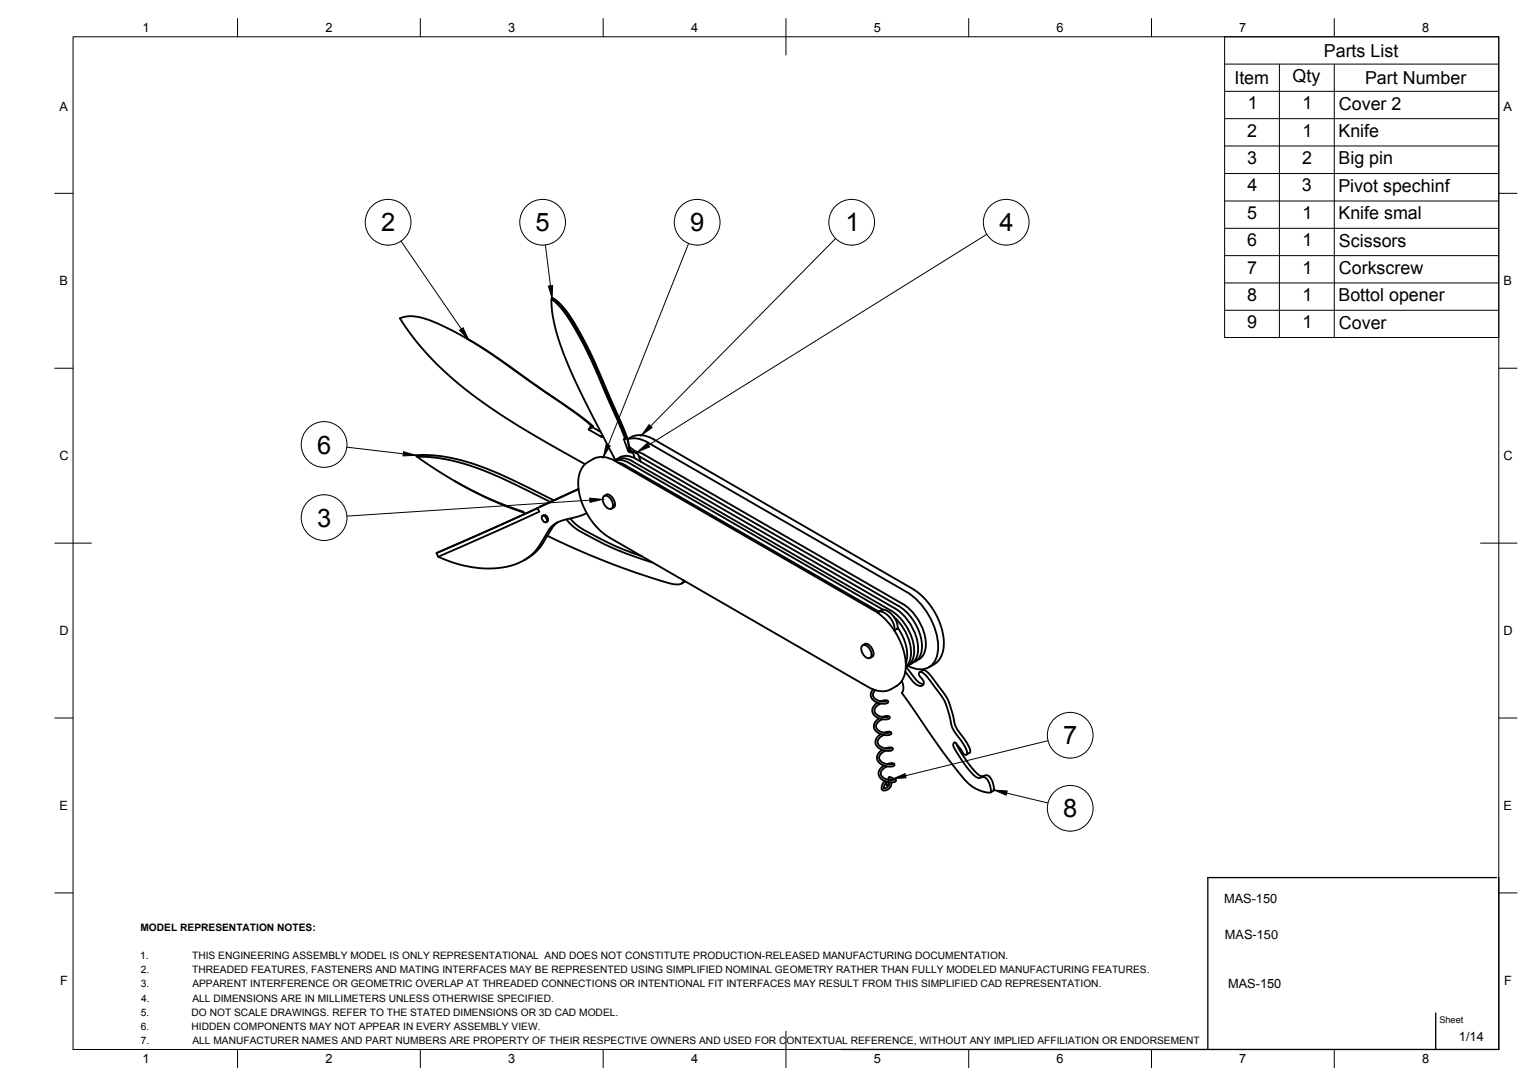
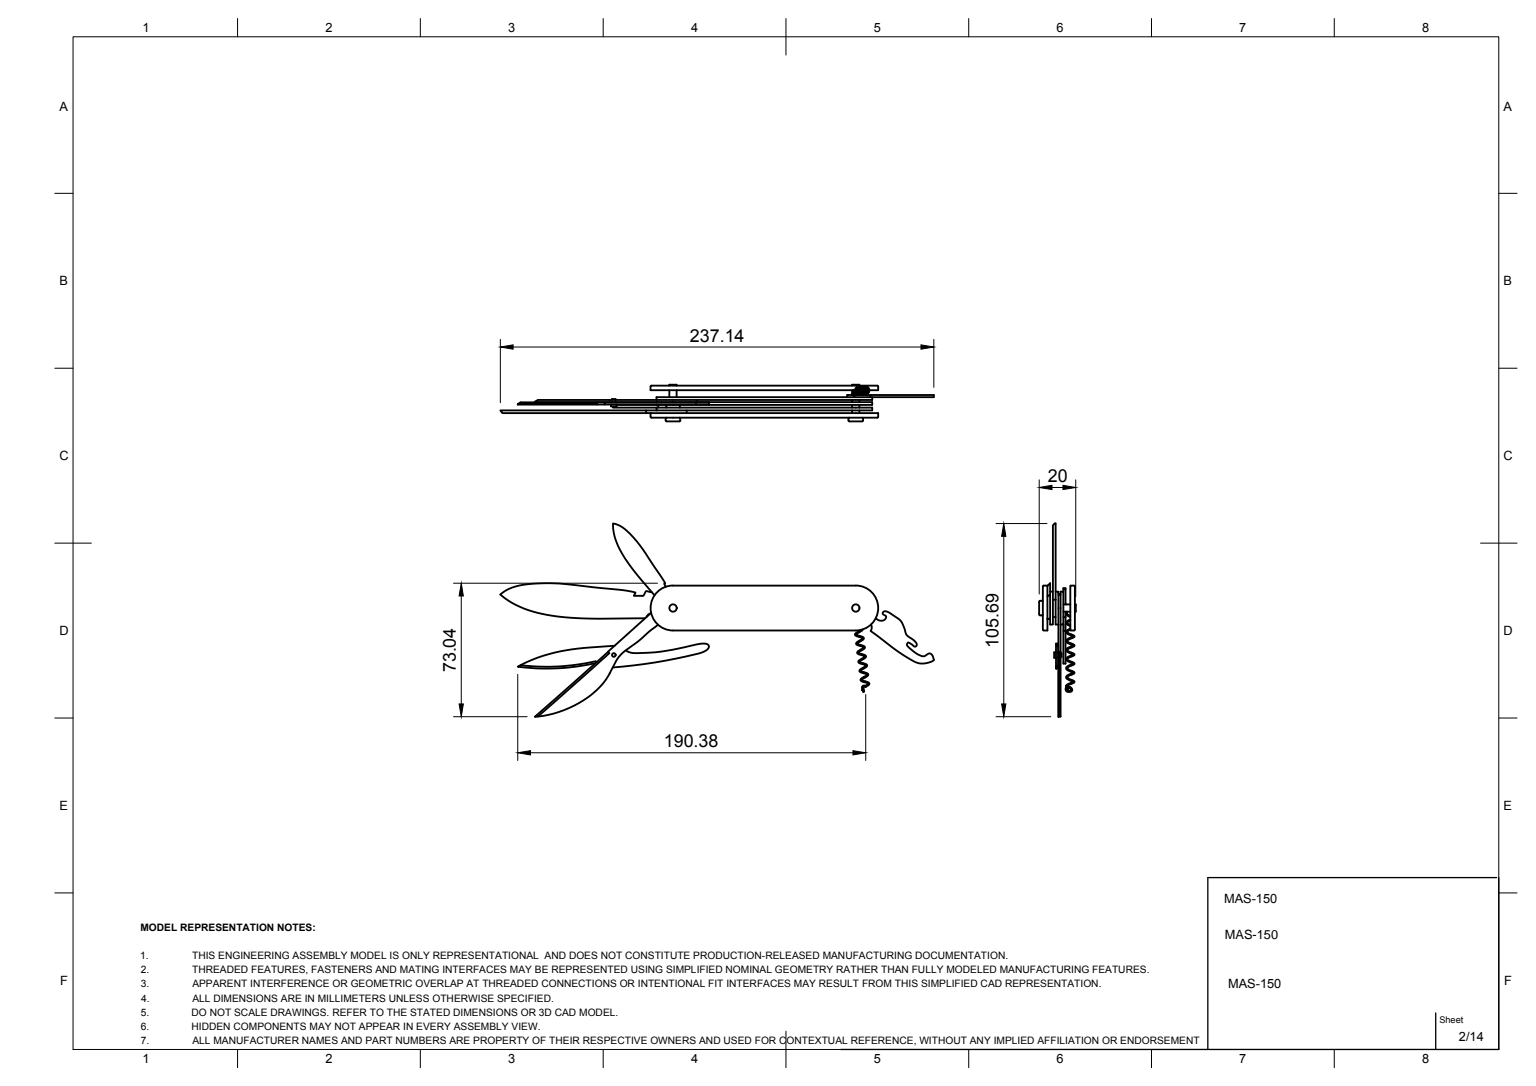
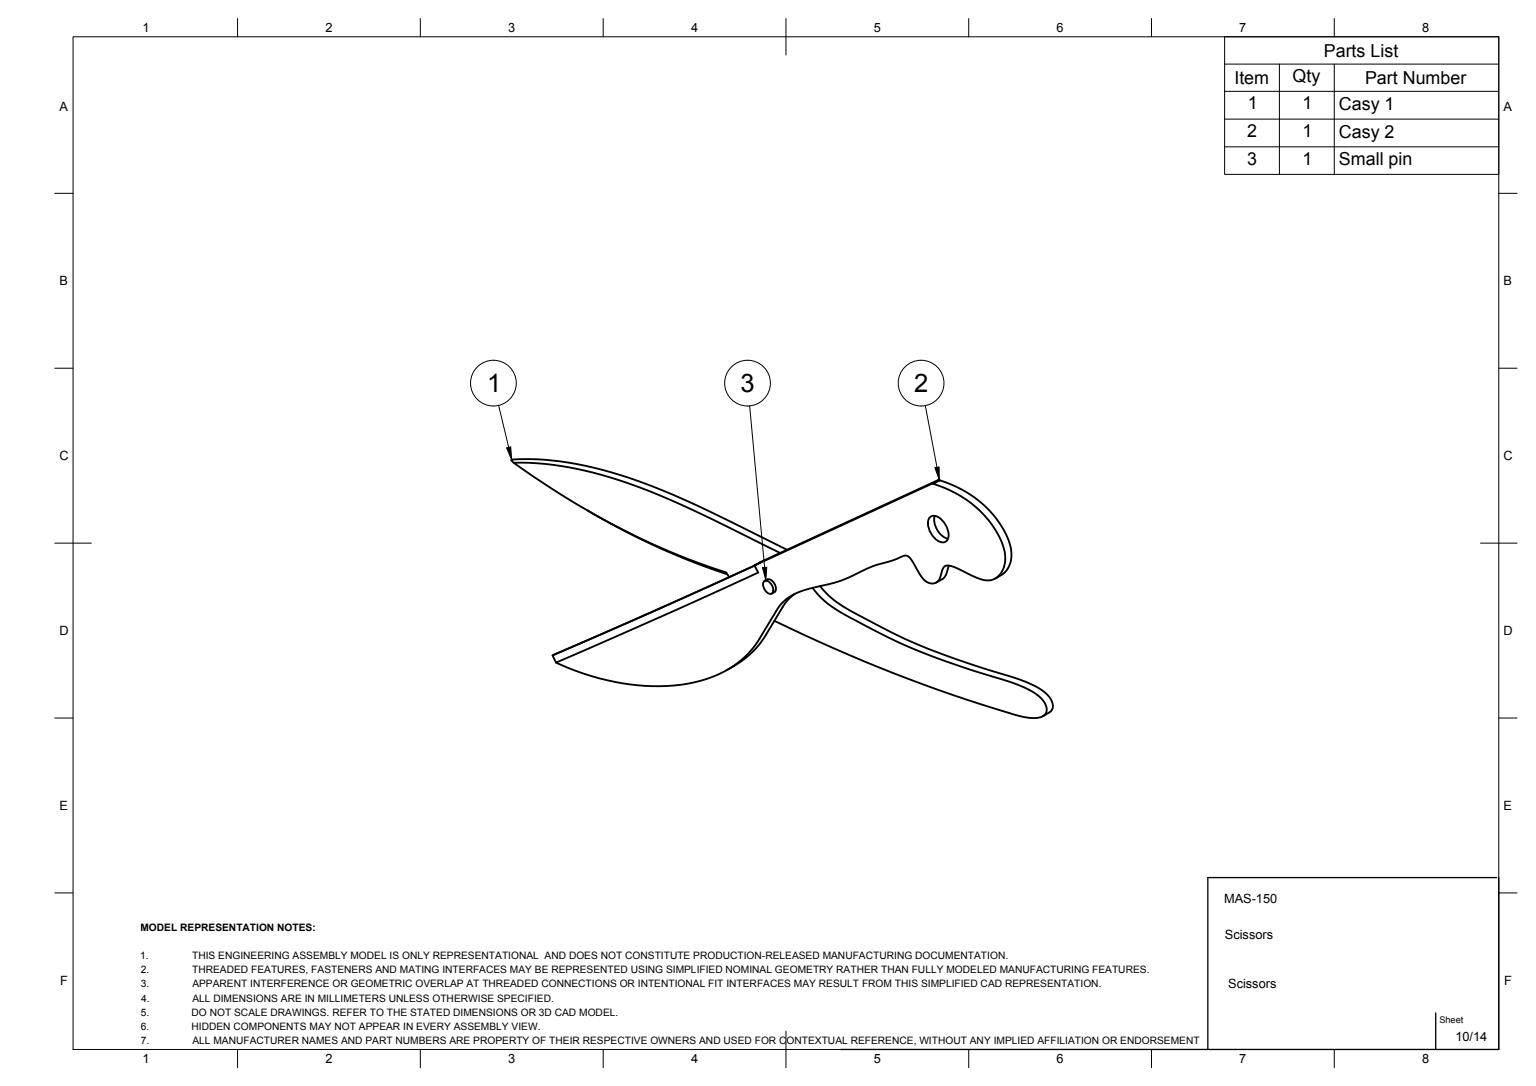
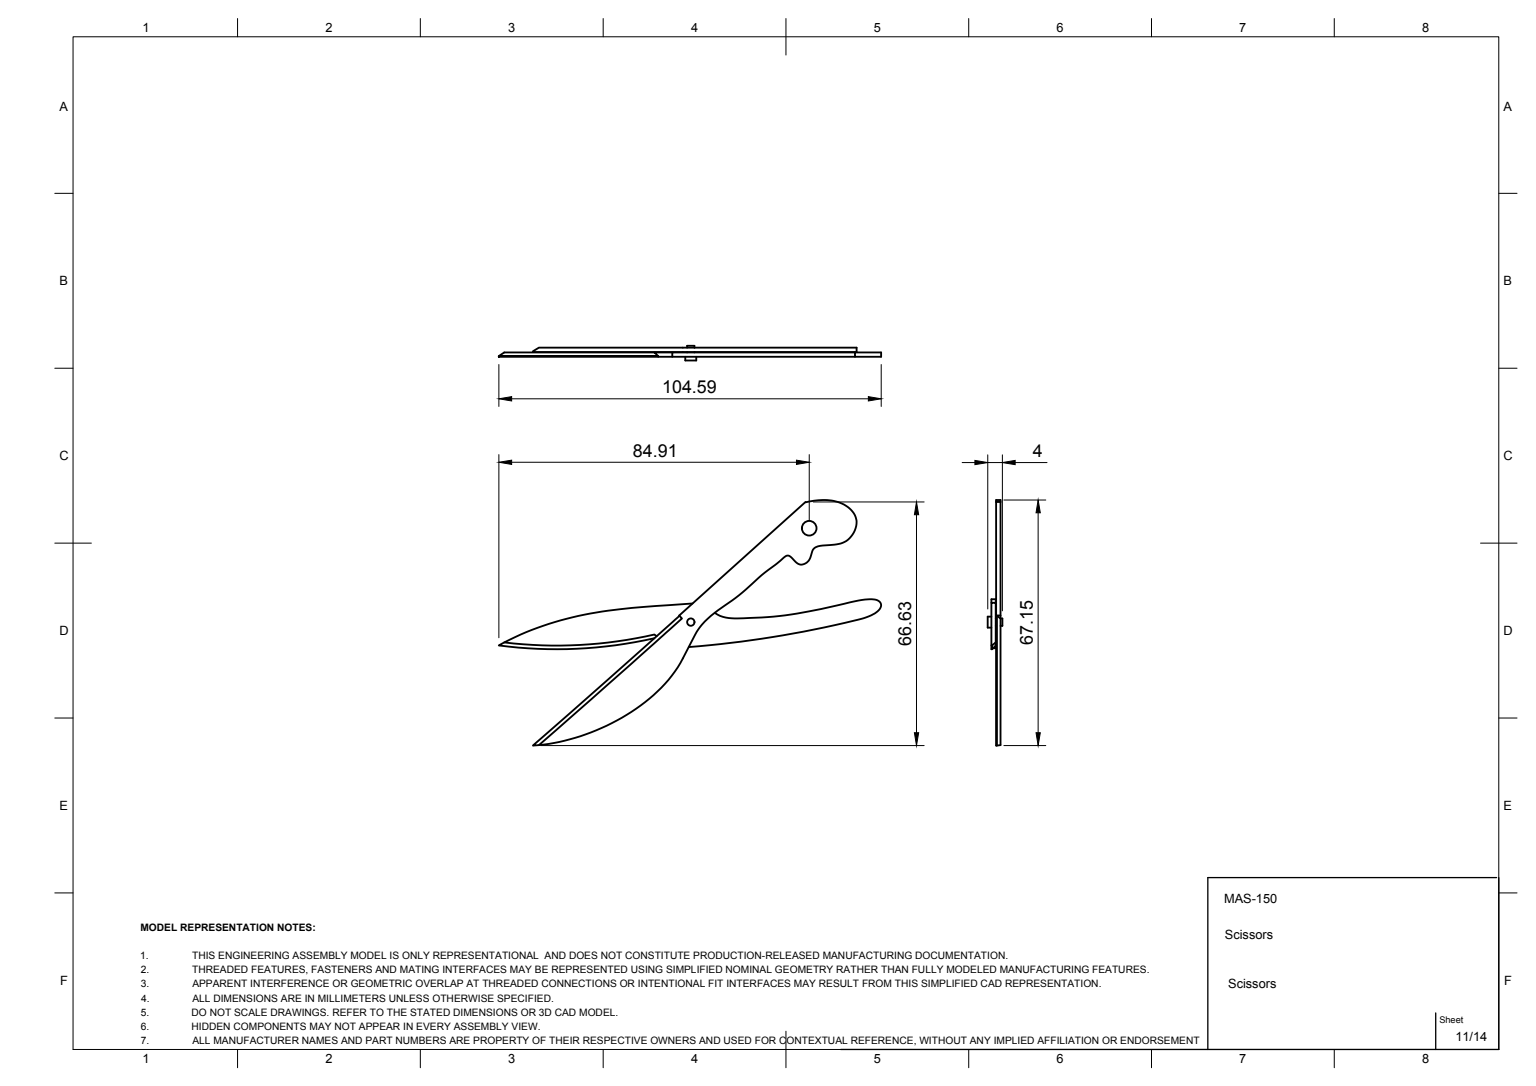
ISO-10303-21;
HEADER;
/* Generated by software containing ST-Developer
 * from STEP Tools, Inc. (www.steptools.com) 
 */

FILE_DESCRIPTION(
/* description */ ('STEP AP203'),
/* implementation_level */ '2;1');

FILE_NAME(
/* name */ 'MAS-150',
/* time_stamp */ '2026-11-08T21:40:52-08:00',
/* author */ (''),
/* organization */ (''),
/* preprocessor_version */ 'ST-DEVELOPER v20.2',
/* originating_system */ 'Autodesk Translation Framework v15.17.0.0',
/* authorisation */ '');

FILE_SCHEMA (('AUTOMOTIVE_DESIGN { 1 0 10303 214 3 1 1 }'));
ENDSEC;

DATA;
#10=MECHANICAL_DESIGN_GEOMETRIC_PRESENTATION_REPRESENTATION('',(#183,#184,
#185,#186,#187,#188,#189,#190,#191,#192,#193),#12137);
#11=(
BOUNDED_CURVE()
B_SPLINE_CURVE(2,(#7724,#7725,#7726,#7727,#7728,#7729,#7730,#7731,#7732,
#7733,#7734,#7735,#7736,#7737,#7738,#7739,#7740,#7741,#7742,#7743,#7744,
#7745,#7746,#7747,#7748,#7749,#7750,#7751,#7752,#7753,#7754,#7755,#7756,
#7757,#7758,#7759,#7760,#7761,#7762,#7763,#7764,#7765,#7766,#7767,#7768,
#7769,#7770,#7771,#7772,#7773,#7774,#7775,#7776,#7777,#7778,#7779,#7780,
#7781,#7782,#7783,#7784,#7785,#7786,#7787,#7788,#7789,#7790,#7791,#7792,
#7793,#7794,#7795,#7796,#7797,#7798,#7799,#7800,#7801,#7802,#7803,#7804,
#7805,#7806,#7807,#7808,#7809,#7810,#7811,#7812,#7813,#7814,#7815,#7816,
#7817,#7818,#7819,#7820,#7821,#7822,#7823,#7824,#7825,#7826,#7827,#7828,
#7829,#7830,#7831,#7832,#7833,#7834,#7835,#7836,#7837,#7838,#7839,#7840,
#7841,#7842,#7843,#7844,#7845,#7846,#7847,#7848,#7849,#7850,#7851,#7852,
#7853,#7854,#7855,#7856,#7857,#7858,#7859,#7860,#7861,#7862,#7863,#7864,
#7865,#7866,#7867,#7868,#7869,#7870,#7871,#7872,#7873,#7874,#7875,#7876,
#7877,#7878,#7879,#7880,#7881,#7882,#7883,#7884,#7885,#7886,#7887,#7888,
#7889,#7890,#7891,#7892,#7893,#7894,#7895,#7896,#7897,#7898,#7899,#7900,
#7901,#7902,#7903,#7904,#7905,#7906,#7907,#7908,#7909,#7910,#7911,#7912,
#7913,#7914,#7915,#7916),.UNSPECIFIED.,.F.,.F.)
B_SPLINE_CURVE_WITH_KNOTS((3,2,2,2,2,2,2,2,2,2,2,2,2,2,2,2,2,2,2,2,2,2,
2,2,2,2,2,2,2,2,2,2,2,2,2,2,2,2,2,2,2,2,2,2,2,2,2,2,2,2,2,2,2,2,2,2,2,2,
2,2,2,2,2,2,2,2,2,2,2,2,2,2,2,2,2,2,2,2,2,2,2,2,2,2,2,2,2,2,2,2,2,2,2,2,
2,2,3),(0.,0.0104166666666667,0.0208333333333333,0.03125,0.0416666666666667,
0.0520833333333333,0.0625,0.0729166666666667,0.0833333333333333,0.09375,
0.104166666666667,0.114583333333333,0.125,0.135416666666667,0.145833333333333,
0.15625,0.166666666666667,0.177083333333333,0.1875,0.197916666666667,0.208333333333333,
0.21875,0.229166666666667,0.239583333333333,0.25,0.260416666666667,0.270833333333333,
0.28125,0.291666666666667,0.302083333333333,0.3125,0.322916666666667,0.333333333333333,
0.34375,0.354166666666667,0.364583333333333,0.375,0.385416666666667,0.395833333333333,
0.40625,0.416666666666667,0.427083333333333,0.4375,0.447916666666667,0.458333333333333,
0.46875,0.479166666666667,0.489583333333333,0.5,0.510416666666667,0.520833333333333,
0.53125,0.541666666666667,0.552083333333333,0.5625,0.572916666666667,0.583333333333333,
0.59375,0.604166666666667,0.614583333333333,0.625,0.635416666666667,0.645833333333333,
0.65625,0.666666666666667,0.677083333333333,0.6875,0.697916666666667,0.708333333333333,
0.71875,0.729166666666667,0.739583333333333,0.75,0.760416666666667,0.770833333333333,
0.78125,0.791666666666667,0.802083333333333,0.8125,0.822916666666667,0.833333333333333,
0.84375,0.854166666666667,0.864583333333333,0.875,0.885416666666667,0.895833333333333,
0.90625,0.916666666666667,0.927083333333333,0.9375,0.947916666666667,0.958333333333333,
0.96875,0.979166666666667,0.989583333333333,1.),.UNSPECIFIED.)
CURVE()
GEOMETRIC_REPRESENTATION_ITEM()
RATIONAL_B_SPLINE_CURVE((1.,0.965925826289068,1.,0.965925826289068,1.,0.965925826289068,
1.,0.965925826289068,1.,0.965925826289068,1.,0.965925826289068,1.,0.965925826289068,
1.,0.965925826289068,1.,0.965925826289068,1.,0.965925826289068,1.,0.965925826289068,
1.,0.965925826289068,1.,0.965925826289068,1.,0.965925826289068,1.,0.965925826289068,
1.,0.965925826289068,1.,0.965925826289068,1.,0.965925826289068,1.,0.965925826289068,
1.,0.965925826289068,1.,0.965925826289068,1.,0.965925826289068,1.,0.965925826289068,
1.,0.965925826289068,1.,0.965925826289068,1.,0.965925826289068,1.,0.965925826289068,
1.,0.965925826289068,1.,0.965925826289068,1.,0.965925826289068,1.,0.965925826289068,
1.,0.965925826289068,1.,0.965925826289068,1.,0.965925826289068,1.,0.965925826289068,
1.,0.965925826289068,1.,0.965925826289068,1.,0.965925826289068,1.,0.965925826289068,
1.,0.965925826289068,1.,0.965925826289068,1.,0.965925826289068,1.,0.965925826289068,
1.,0.965925826289068,1.,0.965925826289068,1.,0.965925826289068,1.,0.965925826289068,
1.,0.965925826289068,1.,0.965925826289068,1.,0.965925826289068,1.,0.965925826289068,
1.,0.965925826289068,1.,0.965925826289068,1.,0.965925826289068,1.,0.965925826289068,
1.,0.965925826289068,1.,0.965925826289068,1.,0.965925826289068,1.,0.965925826289068,
1.,0.965925826289068,1.,0.965925826289068,1.,0.965925826289068,1.,0.965925826289068,
1.,0.965925826289068,1.,0.965925826289068,1.,0.965925826289068,1.,0.965925826289068,
1.,0.965925826289068,1.,0.965925826289068,1.,0.965925826289068,1.,0.965925826289068,
1.,0.965925826289068,1.,0.965925826289068,1.,0.965925826289068,1.,0.965925826289068,
1.,0.965925826289068,1.,0.965925826289068,1.,0.965925826289068,1.,0.965925826289068,
1.,0.965925826289068,1.,0.965925826289068,1.,0.965925826289068,1.,0.965925826289068,
1.,0.965925826289068,1.,0.965925826289068,1.,0.965925826289068,1.,0.965925826289068,
1.,0.965925826289068,1.,0.965925826289068,1.,0.965925826289068,1.,0.965925826289068,
1.,0.965925826289068,1.,0.965925826289068,1.,0.965925826289068,1.,0.965925826289068,
1.,0.965925826289068,1.))
REPRESENTATION_ITEM('')
);
#12=ELLIPSE('',#2055,0.25726333794061,0.250455511407675);
#13=ELLIPSE('',#2061,0.325552151697954,0.297562874271256);
#14=ELLIPSE('',#2064,0.257263338177418,0.250455511570592);
#15=(
BOUNDED_SURFACE()
B_SPLINE_SURFACE(3,3,((#5281,#5282,#5283,#5284,#5285,#5286,#5287,#5288,
#5289,#5290,#5291,#5292),(#5293,#5294,#5295,#5296,#5297,#5298,#5299,#5300,
#5301,#5302,#5303,#5304),(#5305,#5306,#5307,#5308,#5309,#5310,#5311,#5312,
#5313,#5314,#5315,#5316),(#5317,#5318,#5319,#5320,#5321,#5322,#5323,#5324,
#5325,#5326,#5327,#5328),(#5329,#5330,#5331,#5332,#5333,#5334,#5335,#5336,
#5337,#5338,#5339,#5340),(#5341,#5342,#5343,#5344,#5345,#5346,#5347,#5348,
#5349,#5350,#5351,#5352),(#5353,#5354,#5355,#5356,#5357,#5358,#5359,#5360,
#5361,#5362,#5363,#5364)),.UNSPECIFIED.,.T.,.F.,.F.)
B_SPLINE_SURFACE_WITH_KNOTS((4,3,4),(4,2,2,2,2,4),(0.,0.5,1.),(0.727251200985696,
0.761344800862484,0.795438400739272,0.863625600492848,0.931812800246424,
1.),.UNSPECIFIED.)
GEOMETRIC_REPRESENTATION_ITEM()
RATIONAL_B_SPLINE_SURFACE(((1.,1.,1.,1.,1.,1.,1.,1.,1.,1.,1.,1.),(0.333333333333333,
0.333333333333333,0.333333333333333,0.333333333333333,0.333333333333333,
0.333333333333333,0.333333333333333,0.333333333333333,0.333333333333333,
0.333333333333333,0.333333333333333,0.333333333333333),(0.333333333333333,
0.333333333333333,0.333333333333333,0.333333333333333,0.333333333333333,
0.333333333333333,0.333333333333333,0.333333333333333,0.333333333333333,
0.333333333333333,0.333333333333333,0.333333333333333),(1.,1.,1.,1.,1.,
1.,1.,1.,1.,1.,1.,1.),(0.333333333333333,0.333333333333333,0.333333333333333,
0.333333333333333,0.333333333333333,0.333333333333333,0.333333333333333,
0.333333333333333,0.333333333333333,0.333333333333333,0.333333333333333,
0.333333333333333),(0.333333333333333,0.333333333333333,0.333333333333333,
0.333333333333333,0.333333333333333,0.333333333333333,0.333333333333333,
0.333333333333333,0.333333333333333,0.333333333333333,0.333333333333333,
0.333333333333333),(1.,1.,1.,1.,1.,1.,1.,1.,1.,1.,1.,1.)))
REPRESENTATION_ITEM('')
SURFACE()
);
#16=(
BOUNDED_SURFACE()
B_SPLINE_SURFACE(3,3,((#5394,#5395,#5396,#5397,#5398,#5399,#5400,#5401,
#5402,#5403,#5404,#5405,#5406,#5407,#5408,#5409,#5410,#5411,#5412,#5413,
#5414,#5415,#5416,#5417,#5418,#5419,#5420,#5421,#5422,#5423,#5424,#5425,
#5426,#5427,#5428,#5429,#5430,#5431,#5432,#5433),(#5434,#5435,#5436,#5437,
#5438,#5439,#5440,#5441,#5442,#5443,#5444,#5445,#5446,#5447,#5448,#5449,
#5450,#5451,#5452,#5453,#5454,#5455,#5456,#5457,#5458,#5459,#5460,#5461,
#5462,#5463,#5464,#5465,#5466,#5467,#5468,#5469,#5470,#5471,#5472,#5473),
(#5474,#5475,#5476,#5477,#5478,#5479,#5480,#5481,#5482,#5483,#5484,#5485,
#5486,#5487,#5488,#5489,#5490,#5491,#5492,#5493,#5494,#5495,#5496,#5497,
#5498,#5499,#5500,#5501,#5502,#5503,#5504,#5505,#5506,#5507,#5508,#5509,
#5510,#5511,#5512,#5513),(#5514,#5515,#5516,#5517,#5518,#5519,#5520,#5521,
#5522,#5523,#5524,#5525,#5526,#5527,#5528,#5529,#5530,#5531,#5532,#5533,
#5534,#5535,#5536,#5537,#5538,#5539,#5540,#5541,#5542,#5543,#5544,#5545,
#5546,#5547,#5548,#5549,#5550,#5551,#5552,#5553),(#5554,#5555,#5556,#5557,
#5558,#5559,#5560,#5561,#5562,#5563,#5564,#5565,#5566,#5567,#5568,#5569,
#5570,#5571,#5572,#5573,#5574,#5575,#5576,#5577,#5578,#5579,#5580,#5581,
#5582,#5583,#5584,#5585,#5586,#5587,#5588,#5589,#5590,#5591,#5592,#5593),
(#5594,#5595,#5596,#5597,#5598,#5599,#5600,#5601,#5602,#5603,#5604,#5605,
#5606,#5607,#5608,#5609,#5610,#5611,#5612,#5613,#5614,#5615,#5616,#5617,
#5618,#5619,#5620,#5621,#5622,#5623,#5624,#5625,#5626,#5627,#5628,#5629,
#5630,#5631,#5632,#5633),(#5634,#5635,#5636,#5637,#5638,#5639,#5640,#5641,
#5642,#5643,#5644,#5645,#5646,#5647,#5648,#5649,#5650,#5651,#5652,#5653,
#5654,#5655,#5656,#5657,#5658,#5659,#5660,#5661,#5662,#5663,#5664,#5665,
#5666,#5667,#5668,#5669,#5670,#5671,#5672,#5673)),.UNSPECIFIED.,.T.,.F.,
 .F.)
B_SPLINE_SURFACE_WITH_KNOTS((4,3,4),(4,2,2,2,2,2,2,2,2,2,2,2,2,2,2,2,2,
2,2,4),(0.,0.5,1.),(0.,0.0437517296050676,0.0875034592101352,0.131255188815203,
0.17500691842027,0.196882783222804,0.218758648025338,0.262510377630406,
0.350013836840541,0.418185084306465,0.486356331772389,0.554527579238313,
0.622698826704237,0.669861473366207,0.717024120028178,0.811349413352118,
0.858512060014089,0.905674706676059,0.95283735333803,1.),.UNSPECIFIED.)
GEOMETRIC_REPRESENTATION_ITEM()
RATIONAL_B_SPLINE_SURFACE(((1.,1.,1.,1.,1.,1.,1.,1.,1.,1.,1.,1.,1.,1.,1.,
1.,1.,1.,1.,1.,1.,1.,1.,1.,1.,1.,1.,1.,1.,1.,1.,1.,1.,1.,1.,1.,1.,1.,1.,
1.),(0.333333333333333,0.333333333333333,0.333333333333333,0.333333333333333,
0.333333333333333,0.333333333333333,0.333333333333333,0.333333333333333,
0.333333333333333,0.333333333333333,0.333333333333333,0.333333333333333,
0.333333333333333,0.333333333333333,0.333333333333333,0.333333333333333,
0.333333333333333,0.333333333333333,0.333333333333333,0.333333333333333,
0.333333333333333,0.333333333333333,0.333333333333333,0.333333333333333,
0.333333333333333,0.333333333333333,0.333333333333333,0.333333333333333,
0.333333333333333,0.333333333333333,0.333333333333333,0.333333333333333,
0.333333333333333,0.333333333333333,0.333333333333333,0.333333333333333,
0.333333333333333,0.333333333333333,0.333333333333333,0.333333333333333),
(0.333333333333333,0.333333333333333,0.333333333333333,0.333333333333333,
0.333333333333333,0.333333333333333,0.333333333333333,0.333333333333333,
0.333333333333333,0.333333333333333,0.333333333333333,0.333333333333333,
0.333333333333333,0.333333333333333,0.333333333333333,0.333333333333333,
0.333333333333333,0.333333333333333,0.333333333333333,0.333333333333333,
0.333333333333333,0.333333333333333,0.333333333333333,0.333333333333333,
0.333333333333333,0.333333333333333,0.333333333333333,0.333333333333333,
0.333333333333333,0.333333333333333,0.333333333333333,0.333333333333333,
0.333333333333333,0.333333333333333,0.333333333333333,0.333333333333333,
0.333333333333333,0.333333333333333,0.333333333333333,0.333333333333333),
(1.,1.,1.,1.,1.,1.,1.,1.,1.,1.,1.,1.,1.,1.,1.,1.,1.,1.,1.,1.,1.,1.,1.,1.,
1.,1.,1.,1.,1.,1.,1.,1.,1.,1.,1.,1.,1.,1.,1.,1.),(0.333333333333333,0.333333333333333,
0.333333333333333,0.333333333333333,0.333333333333333,0.333333333333333,
0.333333333333333,0.333333333333333,0.333333333333333,0.333333333333333,
0.333333333333333,0.333333333333333,0.333333333333333,0.333333333333333,
0.333333333333333,0.333333333333333,0.333333333333333,0.333333333333333,
0.333333333333333,0.333333333333333,0.333333333333333,0.333333333333333,
0.333333333333333,0.333333333333333,0.333333333333333,0.333333333333333,
0.333333333333333,0.333333333333333,0.333333333333333,0.333333333333333,
0.333333333333333,0.333333333333333,0.333333333333333,0.333333333333333,
0.333333333333333,0.333333333333333,0.333333333333333,0.333333333333333,
0.333333333333333,0.333333333333333),(0.333333333333333,0.333333333333333,
0.333333333333333,0.333333333333333,0.333333333333333,0.333333333333333,
0.333333333333333,0.333333333333333,0.333333333333333,0.333333333333333,
0.333333333333333,0.333333333333333,0.333333333333333,0.333333333333333,
0.333333333333333,0.333333333333333,0.333333333333333,0.333333333333333,
0.333333333333333,0.333333333333333,0.333333333333333,0.333333333333333,
0.333333333333333,0.333333333333333,0.333333333333333,0.333333333333333,
0.333333333333333,0.333333333333333,0.333333333333333,0.333333333333333,
0.333333333333333,0.333333333333333,0.333333333333333,0.333333333333333,
0.333333333333333,0.333333333333333,0.333333333333333,0.333333333333333,
0.333333333333333,0.333333333333333),(1.,1.,1.,1.,1.,1.,1.,1.,1.,1.,1.,
1.,1.,1.,1.,1.,1.,1.,1.,1.,1.,1.,1.,1.,1.,1.,1.,1.,1.,1.,1.,1.,1.,1.,1.,
1.,1.,1.,1.,1.)))
REPRESENTATION_ITEM('')
SURFACE()
);
#17=(
BOUNDED_SURFACE()
B_SPLINE_SURFACE(3,2,((#5791,#5792,#5793,#5794,#5795,#5796,#5797,#5798,
#5799,#5800,#5801,#5802,#5803,#5804,#5805,#5806,#5807,#5808,#5809,#5810,
#5811,#5812,#5813,#5814,#5815,#5816,#5817,#5818,#5819,#5820,#5821,#5822,
#5823,#5824,#5825,#5826,#5827,#5828,#5829,#5830,#5831,#5832,#5833,#5834,
#5835,#5836,#5837,#5838,#5839,#5840,#5841,#5842,#5843,#5844,#5845,#5846,
#5847,#5848,#5849,#5850,#5851,#5852,#5853,#5854,#5855,#5856,#5857,#5858,
#5859,#5860,#5861,#5862,#5863,#5864,#5865,#5866,#5867,#5868,#5869,#5870,
#5871,#5872,#5873,#5874,#5875,#5876,#5877,#5878,#5879,#5880,#5881,#5882,
#5883,#5884,#5885,#5886,#5887,#5888,#5889,#5890,#5891,#5892,#5893,#5894,
#5895,#5896,#5897,#5898,#5899,#5900,#5901,#5902,#5903,#5904,#5905,#5906,
#5907,#5908,#5909,#5910,#5911,#5912,#5913,#5914,#5915,#5916,#5917,#5918,
#5919,#5920,#5921,#5922,#5923,#5924,#5925,#5926,#5927,#5928,#5929,#5930,
#5931,#5932,#5933,#5934,#5935,#5936,#5937,#5938,#5939,#5940,#5941,#5942,
#5943,#5944,#5945,#5946,#5947,#5948,#5949,#5950,#5951,#5952,#5953,#5954,
#5955,#5956,#5957,#5958,#5959,#5960,#5961,#5962,#5963,#5964,#5965,#5966,
#5967,#5968,#5969,#5970,#5971,#5972,#5973,#5974,#5975,#5976,#5977,#5978,
#5979,#5980,#5981,#5982,#5983),(#5984,#5985,#5986,#5987,#5988,#5989,#5990,
#5991,#5992,#5993,#5994,#5995,#5996,#5997,#5998,#5999,#6000,#6001,#6002,
#6003,#6004,#6005,#6006,#6007,#6008,#6009,#6010,#6011,#6012,#6013,#6014,
#6015,#6016,#6017,#6018,#6019,#6020,#6021,#6022,#6023,#6024,#6025,#6026,
#6027,#6028,#6029,#6030,#6031,#6032,#6033,#6034,#6035,#6036,#6037,#6038,
#6039,#6040,#6041,#6042,#6043,#6044,#6045,#6046,#6047,#6048,#6049,#6050,
#6051,#6052,#6053,#6054,#6055,#6056,#6057,#6058,#6059,#6060,#6061,#6062,
#6063,#6064,#6065,#6066,#6067,#6068,#6069,#6070,#6071,#6072,#6073,#6074,
#6075,#6076,#6077,#6078,#6079,#6080,#6081,#6082,#6083,#6084,#6085,#6086,
#6087,#6088,#6089,#6090,#6091,#6092,#6093,#6094,#6095,#6096,#6097,#6098,
#6099,#6100,#6101,#6102,#6103,#6104,#6105,#6106,#6107,#6108,#6109,#6110,
#6111,#6112,#6113,#6114,#6115,#6116,#6117,#6118,#6119,#6120,#6121,#6122,
#6123,#6124,#6125,#6126,#6127,#6128,#6129,#6130,#6131,#6132,#6133,#6134,
#6135,#6136,#6137,#6138,#6139,#6140,#6141,#6142,#6143,#6144,#6145,#6146,
#6147,#6148,#6149,#6150,#6151,#6152,#6153,#6154,#6155,#6156,#6157,#6158,
#6159,#6160,#6161,#6162,#6163,#6164,#6165,#6166,#6167,#6168,#6169,#6170,
#6171,#6172,#6173,#6174,#6175,#6176),(#6177,#6178,#6179,#6180,#6181,#6182,
#6183,#6184,#6185,#6186,#6187,#6188,#6189,#6190,#6191,#6192,#6193,#6194,
#6195,#6196,#6197,#6198,#6199,#6200,#6201,#6202,#6203,#6204,#6205,#6206,
#6207,#6208,#6209,#6210,#6211,#6212,#6213,#6214,#6215,#6216,#6217,#6218,
#6219,#6220,#6221,#6222,#6223,#6224,#6225,#6226,#6227,#6228,#6229,#6230,
#6231,#6232,#6233,#6234,#6235,#6236,#6237,#6238,#6239,#6240,#6241,#6242,
#6243,#6244,#6245,#6246,#6247,#6248,#6249,#6250,#6251,#6252,#6253,#6254,
#6255,#6256,#6257,#6258,#6259,#6260,#6261,#6262,#6263,#6264,#6265,#6266,
#6267,#6268,#6269,#6270,#6271,#6272,#6273,#6274,#6275,#6276,#6277,#6278,
#6279,#6280,#6281,#6282,#6283,#6284,#6285,#6286,#6287,#6288,#6289,#6290,
#6291,#6292,#6293,#6294,#6295,#6296,#6297,#6298,#6299,#6300,#6301,#6302,
#6303,#6304,#6305,#6306,#6307,#6308,#6309,#6310,#6311,#6312,#6313,#6314,
#6315,#6316,#6317,#6318,#6319,#6320,#6321,#6322,#6323,#6324,#6325,#6326,
#6327,#6328,#6329,#6330,#6331,#6332,#6333,#6334,#6335,#6336,#6337,#6338,
#6339,#6340,#6341,#6342,#6343,#6344,#6345,#6346,#6347,#6348,#6349,#6350,
#6351,#6352,#6353,#6354,#6355,#6356,#6357,#6358,#6359,#6360,#6361,#6362,
#6363,#6364,#6365,#6366,#6367,#6368,#6369),(#6370,#6371,#6372,#6373,#6374,
#6375,#6376,#6377,#6378,#6379,#6380,#6381,#6382,#6383,#6384,#6385,#6386,
#6387,#6388,#6389,#6390,#6391,#6392,#6393,#6394,#6395,#6396,#6397,#6398,
#6399,#6400,#6401,#6402,#6403,#6404,#6405,#6406,#6407,#6408,#6409,#6410,
#6411,#6412,#6413,#6414,#6415,#6416,#6417,#6418,#6419,#6420,#6421,#6422,
#6423,#6424,#6425,#6426,#6427,#6428,#6429,#6430,#6431,#6432,#6433,#6434,
#6435,#6436,#6437,#6438,#6439,#6440,#6441,#6442,#6443,#6444,#6445,#6446,
#6447,#6448,#6449,#6450,#6451,#6452,#6453,#6454,#6455,#6456,#6457,#6458,
#6459,#6460,#6461,#6462,#6463,#6464,#6465,#6466,#6467,#6468,#6469,#6470,
#6471,#6472,#6473,#6474,#6475,#6476,#6477,#6478,#6479,#6480,#6481,#6482,
#6483,#6484,#6485,#6486,#6487,#6488,#6489,#6490,#6491,#6492,#6493,#6494,
#6495,#6496,#6497,#6498,#6499,#6500,#6501,#6502,#6503,#6504,#6505,#6506,
#6507,#6508,#6509,#6510,#6511,#6512,#6513,#6514,#6515,#6516,#6517,#6518,
#6519,#6520,#6521,#6522,#6523,#6524,#6525,#6526,#6527,#6528,#6529,#6530,
#6531,#6532,#6533,#6534,#6535,#6536,#6537,#6538,#6539,#6540,#6541,#6542,
#6543,#6544,#6545,#6546,#6547,#6548,#6549,#6550,#6551,#6552,#6553,#6554,
#6555,#6556,#6557,#6558,#6559,#6560,#6561,#6562),(#6563,#6564,#6565,#6566,
#6567,#6568,#6569,#6570,#6571,#6572,#6573,#6574,#6575,#6576,#6577,#6578,
#6579,#6580,#6581,#6582,#6583,#6584,#6585,#6586,#6587,#6588,#6589,#6590,
#6591,#6592,#6593,#6594,#6595,#6596,#6597,#6598,#6599,#6600,#6601,#6602,
#6603,#6604,#6605,#6606,#6607,#6608,#6609,#6610,#6611,#6612,#6613,#6614,
#6615,#6616,#6617,#6618,#6619,#6620,#6621,#6622,#6623,#6624,#6625,#6626,
#6627,#6628,#6629,#6630,#6631,#6632,#6633,#6634,#6635,#6636,#6637,#6638,
#6639,#6640,#6641,#6642,#6643,#6644,#6645,#6646,#6647,#6648,#6649,#6650,
#6651,#6652,#6653,#6654,#6655,#6656,#6657,#6658,#6659,#6660,#6661,#6662,
#6663,#6664,#6665,#6666,#6667,#6668,#6669,#6670,#6671,#6672,#6673,#6674,
#6675,#6676,#6677,#6678,#6679,#6680,#6681,#6682,#6683,#6684,#6685,#6686,
#6687,#6688,#6689,#6690,#6691,#6692,#6693,#6694,#6695,#6696,#6697,#6698,
#6699,#6700,#6701,#6702,#6703,#6704,#6705,#6706,#6707,#6708,#6709,#6710,
#6711,#6712,#6713,#6714,#6715,#6716,#6717,#6718,#6719,#6720,#6721,#6722,
#6723,#6724,#6725,#6726,#6727,#6728,#6729,#6730,#6731,#6732,#6733,#6734,
#6735,#6736,#6737,#6738,#6739,#6740,#6741,#6742,#6743,#6744,#6745,#6746,
#6747,#6748,#6749,#6750,#6751,#6752,#6753,#6754,#6755),(#6756,#6757,#6758,
#6759,#6760,#6761,#6762,#6763,#6764,#6765,#6766,#6767,#6768,#6769,#6770,
#6771,#6772,#6773,#6774,#6775,#6776,#6777,#6778,#6779,#6780,#6781,#6782,
#6783,#6784,#6785,#6786,#6787,#6788,#6789,#6790,#6791,#6792,#6793,#6794,
#6795,#6796,#6797,#6798,#6799,#6800,#6801,#6802,#6803,#6804,#6805,#6806,
#6807,#6808,#6809,#6810,#6811,#6812,#6813,#6814,#6815,#6816,#6817,#6818,
#6819,#6820,#6821,#6822,#6823,#6824,#6825,#6826,#6827,#6828,#6829,#6830,
#6831,#6832,#6833,#6834,#6835,#6836,#6837,#6838,#6839,#6840,#6841,#6842,
#6843,#6844,#6845,#6846,#6847,#6848,#6849,#6850,#6851,#6852,#6853,#6854,
#6855,#6856,#6857,#6858,#6859,#6860,#6861,#6862,#6863,#6864,#6865,#6866,
#6867,#6868,#6869,#6870,#6871,#6872,#6873,#6874,#6875,#6876,#6877,#6878,
#6879,#6880,#6881,#6882,#6883,#6884,#6885,#6886,#6887,#6888,#6889,#6890,
#6891,#6892,#6893,#6894,#6895,#6896,#6897,#6898,#6899,#6900,#6901,#6902,
#6903,#6904,#6905,#6906,#6907,#6908,#6909,#6910,#6911,#6912,#6913,#6914,
#6915,#6916,#6917,#6918,#6919,#6920,#6921,#6922,#6923,#6924,#6925,#6926,
#6927,#6928,#6929,#6930,#6931,#6932,#6933,#6934,#6935,#6936,#6937,#6938,
#6939,#6940,#6941,#6942,#6943,#6944,#6945,#6946,#6947,#6948),(#6949,#6950,
#6951,#6952,#6953,#6954,#6955,#6956,#6957,#6958,#6959,#6960,#6961,#6962,
#6963,#6964,#6965,#6966,#6967,#6968,#6969,#6970,#6971,#6972,#6973,#6974,
#6975,#6976,#6977,#6978,#6979,#6980,#6981,#6982,#6983,#6984,#6985,#6986,
#6987,#6988,#6989,#6990,#6991,#6992,#6993,#6994,#6995,#6996,#6997,#6998,
#6999,#7000,#7001,#7002,#7003,#7004,#7005,#7006,#7007,#7008,#7009,#7010,
#7011,#7012,#7013,#7014,#7015,#7016,#7017,#7018,#7019,#7020,#7021,#7022,
#7023,#7024,#7025,#7026,#7027,#7028,#7029,#7030,#7031,#7032,#7033,#7034,
#7035,#7036,#7037,#7038,#7039,#7040,#7041,#7042,#7043,#7044,#7045,#7046,
#7047,#7048,#7049,#7050,#7051,#7052,#7053,#7054,#7055,#7056,#7057,#7058,
#7059,#7060,#7061,#7062,#7063,#7064,#7065,#7066,#7067,#7068,#7069,#7070,
#7071,#7072,#7073,#7074,#7075,#7076,#7077,#7078,#7079,#7080,#7081,#7082,
#7083,#7084,#7085,#7086,#7087,#7088,#7089,#7090,#7091,#7092,#7093,#7094,
#7095,#7096,#7097,#7098,#7099,#7100,#7101,#7102,#7103,#7104,#7105,#7106,
#7107,#7108,#7109,#7110,#7111,#7112,#7113,#7114,#7115,#7116,#7117,#7118,
#7119,#7120,#7121,#7122,#7123,#7124,#7125,#7126,#7127,#7128,#7129,#7130,
#7131,#7132,#7133,#7134,#7135,#7136,#7137,#7138,#7139,#7140,#7141),(#7142,
#7143,#7144,#7145,#7146,#7147,#7148,#7149,#7150,#7151,#7152,#7153,#7154,
#7155,#7156,#7157,#7158,#7159,#7160,#7161,#7162,#7163,#7164,#7165,#7166,
#7167,#7168,#7169,#7170,#7171,#7172,#7173,#7174,#7175,#7176,#7177,#7178,
#7179,#7180,#7181,#7182,#7183,#7184,#7185,#7186,#7187,#7188,#7189,#7190,
#7191,#7192,#7193,#7194,#7195,#7196,#7197,#7198,#7199,#7200,#7201,#7202,
#7203,#7204,#7205,#7206,#7207,#7208,#7209,#7210,#7211,#7212,#7213,#7214,
#7215,#7216,#7217,#7218,#7219,#7220,#7221,#7222,#7223,#7224,#7225,#7226,
#7227,#7228,#7229,#7230,#7231,#7232,#7233,#7234,#7235,#7236,#7237,#7238,
#7239,#7240,#7241,#7242,#7243,#7244,#7245,#7246,#7247,#7248,#7249,#7250,
#7251,#7252,#7253,#7254,#7255,#7256,#7257,#7258,#7259,#7260,#7261,#7262,
#7263,#7264,#7265,#7266,#7267,#7268,#7269,#7270,#7271,#7272,#7273,#7274,
#7275,#7276,#7277,#7278,#7279,#7280,#7281,#7282,#7283,#7284,#7285,#7286,
#7287,#7288,#7289,#7290,#7291,#7292,#7293,#7294,#7295,#7296,#7297,#7298,
#7299,#7300,#7301,#7302,#7303,#7304,#7305,#7306,#7307,#7308,#7309,#7310,
#7311,#7312,#7313,#7314,#7315,#7316,#7317,#7318,#7319,#7320,#7321,#7322,
#7323,#7324,#7325,#7326,#7327,#7328,#7329,#7330,#7331,#7332,#7333,#7334),
(#7335,#7336,#7337,#7338,#7339,#7340,#7341,#7342,#7343,#7344,#7345,#7346,
#7347,#7348,#7349,#7350,#7351,#7352,#7353,#7354,#7355,#7356,#7357,#7358,
#7359,#7360,#7361,#7362,#7363,#7364,#7365,#7366,#7367,#7368,#7369,#7370,
#7371,#7372,#7373,#7374,#7375,#7376,#7377,#7378,#7379,#7380,#7381,#7382,
#7383,#7384,#7385,#7386,#7387,#7388,#7389,#7390,#7391,#7392,#7393,#7394,
#7395,#7396,#7397,#7398,#7399,#7400,#7401,#7402,#7403,#7404,#7405,#7406,
#7407,#7408,#7409,#7410,#7411,#7412,#7413,#7414,#7415,#7416,#7417,#7418,
#7419,#7420,#7421,#7422,#7423,#7424,#7425,#7426,#7427,#7428,#7429,#7430,
#7431,#7432,#7433,#7434,#7435,#7436,#7437,#7438,#7439,#7440,#7441,#7442,
#7443,#7444,#7445,#7446,#7447,#7448,#7449,#7450,#7451,#7452,#7453,#7454,
#7455,#7456,#7457,#7458,#7459,#7460,#7461,#7462,#7463,#7464,#7465,#7466,
#7467,#7468,#7469,#7470,#7471,#7472,#7473,#7474,#7475,#7476,#7477,#7478,
#7479,#7480,#7481,#7482,#7483,#7484,#7485,#7486,#7487,#7488,#7489,#7490,
#7491,#7492,#7493,#7494,#7495,#7496,#7497,#7498,#7499,#7500,#7501,#7502,
#7503,#7504,#7505,#7506,#7507,#7508,#7509,#7510,#7511,#7512,#7513,#7514,
#7515,#7516,#7517,#7518,#7519,#7520,#7521,#7522,#7523,#7524,#7525,#7526,
#7527),(#7528,#7529,#7530,#7531,#7532,#7533,#7534,#7535,#7536,#7537,#7538,
#7539,#7540,#7541,#7542,#7543,#7544,#7545,#7546,#7547,#7548,#7549,#7550,
#7551,#7552,#7553,#7554,#7555,#7556,#7557,#7558,#7559,#7560,#7561,#7562,
#7563,#7564,#7565,#7566,#7567,#7568,#7569,#7570,#7571,#7572,#7573,#7574,
#7575,#7576,#7577,#7578,#7579,#7580,#7581,#7582,#7583,#7584,#7585,#7586,
#7587,#7588,#7589,#7590,#7591,#7592,#7593,#7594,#7595,#7596,#7597,#7598,
#7599,#7600,#7601,#7602,#7603,#7604,#7605,#7606,#7607,#7608,#7609,#7610,
#7611,#7612,#7613,#7614,#7615,#7616,#7617,#7618,#7619,#7620,#7621,#7622,
#7623,#7624,#7625,#7626,#7627,#7628,#7629,#7630,#7631,#7632,#7633,#7634,
#7635,#7636,#7637,#7638,#7639,#7640,#7641,#7642,#7643,#7644,#7645,#7646,
#7647,#7648,#7649,#7650,#7651,#7652,#7653,#7654,#7655,#7656,#7657,#7658,
#7659,#7660,#7661,#7662,#7663,#7664,#7665,#7666,#7667,#7668,#7669,#7670,
#7671,#7672,#7673,#7674,#7675,#7676,#7677,#7678,#7679,#7680,#7681,#7682,
#7683,#7684,#7685,#7686,#7687,#7688,#7689,#7690,#7691,#7692,#7693,#7694,
#7695,#7696,#7697,#7698,#7699,#7700,#7701,#7702,#7703,#7704,#7705,#7706,
#7707,#7708,#7709,#7710,#7711,#7712,#7713,#7714,#7715,#7716,#7717,#7718,
#7719,#7720)),.UNSPECIFIED.,.T.,.F.,.F.)
B_SPLINE_SURFACE_WITH_KNOTS((4,3,3,4),(3,2,2,2,2,2,2,2,2,2,2,2,2,2,2,2,
2,2,2,2,2,2,2,2,2,2,2,2,2,2,2,2,2,2,2,2,2,2,2,2,2,2,2,2,2,2,2,2,2,2,2,2,
2,2,2,2,2,2,2,2,2,2,2,2,2,2,2,2,2,2,2,2,2,2,2,2,2,2,2,2,2,2,2,2,2,2,2,2,
2,2,2,2,2,2,2,2,3),(-5.30788478853017E-5,0.,0.5,0.999946921152115),(0.,
0.0104166666666667,0.0208333333333333,0.03125,0.0416666666666667,0.0520833333333333,
0.0625,0.0729166666666667,0.0833333333333333,0.09375,0.104166666666667,
0.114583333333333,0.125,0.135416666666667,0.145833333333333,0.15625,0.166666666666667,
0.177083333333333,0.1875,0.197916666666667,0.208333333333333,0.21875,0.229166666666667,
0.239583333333333,0.25,0.260416666666667,0.270833333333333,0.28125,0.291666666666667,
0.302083333333333,0.3125,0.322916666666667,0.333333333333333,0.34375,0.354166666666667,
0.364583333333333,0.375,0.385416666666667,0.395833333333333,0.40625,0.416666666666667,
0.427083333333333,0.4375,0.447916666666667,0.458333333333333,0.46875,0.479166666666667,
0.489583333333333,0.5,0.510416666666667,0.520833333333333,0.53125,0.541666666666667,
0.552083333333333,0.5625,0.572916666666667,0.583333333333333,0.59375,0.604166666666667,
0.614583333333333,0.625,0.635416666666667,0.645833333333333,0.65625,0.666666666666667,
0.677083333333333,0.6875,0.697916666666667,0.708333333333333,0.71875,0.729166666666667,
0.739583333333333,0.75,0.760416666666667,0.770833333333333,0.78125,0.791666666666667,
0.802083333333333,0.8125,0.822916666666667,0.833333333333333,0.84375,0.854166666666667,
0.864583333333333,0.875,0.885416666666667,0.895833333333333,0.90625,0.916666666666667,
0.927083333333333,0.9375,0.947916666666667,0.958333333333333,0.96875,0.979166666666667,
0.989583333333333,1.),.UNSPECIFIED.)
GEOMETRIC_REPRESENTATION_ITEM()
RATIONAL_B_SPLINE_SURFACE(((0.999787707147372,0.965720767139978,0.999787707147372,
0.965720767139978,0.999787707147372,0.965720767139978,0.999787707147372,
0.965720767139978,0.999787707147372,0.965720767139978,0.999787707147372,
0.965720767139978,0.999787707147372,0.965720767139978,0.999787707147372,
0.965720767139978,0.999787707147372,0.965720767139978,0.999787707147372,
0.965720767139978,0.999787707147372,0.965720767139978,0.999787707147372,
0.965720767139978,0.999787707147372,0.965720767139978,0.999787707147372,
0.965720767139978,0.999787707147372,0.965720767139978,0.999787707147372,
0.965720767139978,0.999787707147372,0.965720767139978,0.999787707147372,
0.965720767139978,0.999787707147372,0.965720767139978,0.999787707147372,
0.965720767139978,0.999787707147372,0.965720767139978,0.999787707147372,
0.965720767139978,0.999787707147372,0.965720767139978,0.999787707147372,
0.965720767139978,0.999787707147372,0.965720767139978,0.999787707147372,
0.965720767139978,0.999787707147372,0.965720767139978,0.999787707147372,
0.965720767139978,0.999787707147372,0.965720767139978,0.999787707147372,
0.965720767139978,0.999787707147372,0.965720767139978,0.999787707147372,
0.965720767139978,0.999787707147372,0.965720767139978,0.999787707147372,
0.965720767139978,0.999787707147372,0.965720767139978,0.999787707147372,
0.965720767139978,0.999787707147372,0.965720767139978,0.999787707147372,
0.965720767139978,0.999787707147372,0.965720767139978,0.999787707147372,
0.965720767139978,0.999787707147372,0.965720767139978,0.999787707147372,
0.965720767139978,0.999787707147372,0.965720767139978,0.999787707147372,
0.965720767139978,0.999787707147372,0.965720767139978,0.999787707147372,
0.965720767139978,0.999787707147372,0.965720767139978,0.999787707147372,
0.965720767139978,0.999787707147372,0.965720767139978,0.999787707147372,
0.965720767139978,0.999787707147372,0.965720767139978,0.999787707147372,
0.965720767139978,0.999787707147372,0.965720767139978,0.999787707147372,
0.965720767139978,0.999787707147372,0.965720767139978,0.999787707147372,
0.965720767139978,0.999787707147372,0.965720767139978,0.999787707147372,
0.965720767139978,0.999787707147372,0.965720767139978,0.999787707147372,
0.965720767139978,0.999787707147372,0.965720767139978,0.999787707147372,
0.965720767139978,0.999787707147372,0.965720767139978,0.999787707147372,
0.965720767139978,0.999787707147372,0.965720767139978,0.999787707147372,
0.965720767139978,0.999787707147372,0.965720767139978,0.999787707147372,
0.965720767139978,0.999787707147372,0.965720767139978,0.999787707147372,
0.965720767139978,0.999787707147372,0.965720767139978,0.999787707147372,
0.965720767139978,0.999787707147372,0.965720767139978,0.999787707147372,
0.965720767139978,0.999787707147372,0.965720767139978,0.999787707147372,
0.965720767139978,0.999787707147372,0.965720767139978,0.999787707147372,
0.965720767139978,0.999787707147372,0.965720767139978,0.999787707147372,
0.965720767139978,0.999787707147372,0.965720767139978,0.999787707147372,
0.965720767139978,0.999787707147372,0.965720767139978,0.999787707147372,
0.965720767139978,0.999787707147372,0.965720767139978,0.999787707147372,
0.965720767139978,0.999787707147372,0.965720767139978,0.999787707147372,
0.965720767139978,0.999787707147372,0.965720767139978,0.999787707147372,
0.965720767139978,0.999787707147372,0.965720767139978,0.999787707147372,
0.965720767139978,0.999787707147372,0.965720767139978,0.999787707147372,
0.965720767139978,0.999787707147372,0.965720767139978,0.999787707147372,
0.965720767139978,0.999787707147372),(0.99985846391861,0.965789112932702,
0.99985846391861,0.965789112932702,0.99985846391861,0.965789112932702,0.99985846391861,
0.965789112932702,0.99985846391861,0.965789112932702,0.99985846391861,0.965789112932702,
0.99985846391861,0.965789112932702,0.99985846391861,0.965789112932702,0.99985846391861,
0.965789112932702,0.99985846391861,0.965789112932702,0.99985846391861,0.965789112932702,
0.99985846391861,0.965789112932702,0.99985846391861,0.965789112932702,0.99985846391861,
0.965789112932702,0.99985846391861,0.965789112932702,0.99985846391861,0.965789112932702,
0.99985846391861,0.965789112932702,0.99985846391861,0.965789112932702,0.99985846391861,
0.965789112932702,0.99985846391861,0.965789112932702,0.99985846391861,0.965789112932702,
0.99985846391861,0.965789112932702,0.99985846391861,0.965789112932702,0.99985846391861,
0.965789112932702,0.99985846391861,0.965789112932702,0.99985846391861,0.965789112932702,
0.99985846391861,0.965789112932702,0.99985846391861,0.965789112932702,0.99985846391861,
0.965789112932702,0.99985846391861,0.965789112932702,0.99985846391861,0.965789112932702,
0.99985846391861,0.965789112932702,0.99985846391861,0.965789112932702,0.99985846391861,
0.965789112932702,0.99985846391861,0.965789112932702,0.99985846391861,0.965789112932702,
0.99985846391861,0.965789112932702,0.99985846391861,0.965789112932702,0.99985846391861,
0.965789112932702,0.99985846391861,0.965789112932702,0.99985846391861,0.965789112932702,
0.99985846391861,0.965789112932702,0.99985846391861,0.965789112932702,0.99985846391861,
0.965789112932702,0.99985846391861,0.965789112932702,0.99985846391861,0.965789112932702,
0.99985846391861,0.965789112932702,0.99985846391861,0.965789112932702,0.99985846391861,
0.965789112932702,0.99985846391861,0.965789112932702,0.99985846391861,0.965789112932702,
0.99985846391861,0.965789112932702,0.99985846391861,0.965789112932702,0.99985846391861,
0.965789112932702,0.99985846391861,0.965789112932702,0.99985846391861,0.965789112932702,
0.99985846391861,0.965789112932702,0.99985846391861,0.965789112932702,0.99985846391861,
0.965789112932702,0.99985846391861,0.965789112932702,0.99985846391861,0.965789112932702,
0.99985846391861,0.965789112932702,0.99985846391861,0.965789112932702,0.99985846391861,
0.965789112932702,0.99985846391861,0.965789112932702,0.99985846391861,0.965789112932702,
0.99985846391861,0.965789112932702,0.99985846391861,0.965789112932702,0.99985846391861,
0.965789112932702,0.99985846391861,0.965789112932702,0.99985846391861,0.965789112932702,
0.99985846391861,0.965789112932702,0.99985846391861,0.965789112932702,0.99985846391861,
0.965789112932702,0.99985846391861,0.965789112932702,0.99985846391861,0.965789112932702,
0.99985846391861,0.965789112932702,0.99985846391861,0.965789112932702,0.99985846391861,
0.965789112932702,0.99985846391861,0.965789112932702,0.99985846391861,0.965789112932702,
0.99985846391861,0.965789112932702,0.99985846391861,0.965789112932702,0.99985846391861,
0.965789112932702,0.99985846391861,0.965789112932702,0.99985846391861,0.965789112932702,
0.99985846391861,0.965789112932702,0.99985846391861,0.965789112932702,0.99985846391861,
0.965789112932702,0.99985846391861,0.965789112932702,0.99985846391861,0.965789112932702,
0.99985846391861,0.965789112932702,0.99985846391861,0.965789112932702,0.99985846391861,
0.965789112932702,0.99985846391861,0.965789112932702,0.99985846391861,0.965789112932702,
0.99985846391861),(0.99992922820282,0.965857465982399,0.99992922820282,
0.965857465982399,0.99992922820282,0.965857465982399,0.99992922820282,0.965857465982399,
0.99992922820282,0.965857465982399,0.99992922820282,0.965857465982399,0.99992922820282,
0.965857465982399,0.99992922820282,0.965857465982399,0.99992922820282,0.965857465982399,
0.99992922820282,0.965857465982399,0.99992922820282,0.965857465982399,0.99992922820282,
0.965857465982399,0.99992922820282,0.965857465982399,0.99992922820282,0.965857465982399,
0.99992922820282,0.965857465982399,0.99992922820282,0.965857465982399,0.99992922820282,
0.965857465982399,0.99992922820282,0.965857465982399,0.99992922820282,0.965857465982399,
0.99992922820282,0.965857465982399,0.99992922820282,0.965857465982399,0.99992922820282,
0.965857465982399,0.99992922820282,0.965857465982399,0.99992922820282,0.965857465982399,
0.99992922820282,0.965857465982399,0.99992922820282,0.965857465982399,0.99992922820282,
0.965857465982399,0.99992922820282,0.965857465982399,0.99992922820282,0.965857465982399,
0.99992922820282,0.965857465982399,0.99992922820282,0.965857465982399,0.99992922820282,
0.965857465982399,0.99992922820282,0.965857465982399,0.99992922820282,0.965857465982399,
0.99992922820282,0.965857465982399,0.99992922820282,0.965857465982399,0.99992922820282,
0.965857465982399,0.99992922820282,0.965857465982399,0.99992922820282,0.965857465982399,
0.99992922820282,0.965857465982399,0.99992922820282,0.965857465982399,0.99992922820282,
0.965857465982399,0.99992922820282,0.965857465982399,0.99992922820282,0.965857465982399,
0.99992922820282,0.965857465982399,0.99992922820282,0.965857465982399,0.99992922820282,
0.965857465982399,0.99992922820282,0.965857465982399,0.99992922820282,0.965857465982399,
0.99992922820282,0.965857465982399,0.99992922820282,0.965857465982399,0.99992922820282,
0.965857465982399,0.99992922820282,0.965857465982399,0.99992922820282,0.965857465982399,
0.99992922820282,0.965857465982399,0.99992922820282,0.965857465982399,0.99992922820282,
0.965857465982399,0.99992922820282,0.965857465982399,0.99992922820282,0.965857465982399,
0.99992922820282,0.965857465982399,0.99992922820282,0.965857465982399,0.99992922820282,
0.965857465982399,0.99992922820282,0.965857465982399,0.99992922820282,0.965857465982399,
0.99992922820282,0.965857465982399,0.99992922820282,0.965857465982399,0.99992922820282,
0.965857465982399,0.99992922820282,0.965857465982399,0.99992922820282,0.965857465982399,
0.99992922820282,0.965857465982399,0.99992922820282,0.965857465982399,0.99992922820282,
0.965857465982399,0.99992922820282,0.965857465982399,0.99992922820282,0.965857465982399,
0.99992922820282,0.965857465982399,0.99992922820282,0.965857465982399,0.99992922820282,
0.965857465982399,0.99992922820282,0.965857465982399,0.99992922820282,0.965857465982399,
0.99992922820282,0.965857465982399,0.99992922820282,0.965857465982399,0.99992922820282,
0.965857465982399,0.99992922820282,0.965857465982399,0.99992922820282,0.965857465982399,
0.99992922820282,0.965857465982399,0.99992922820282,0.965857465982399,0.99992922820282,
0.965857465982399,0.99992922820282,0.965857465982399,0.99992922820282,0.965857465982399,
0.99992922820282,0.965857465982399,0.99992922820282,0.965857465982399,0.99992922820282,
0.965857465982399,0.99992922820282,0.965857465982399,0.99992922820282,0.965857465982399,
0.99992922820282,0.965857465982399,0.99992922820282,0.965857465982399,0.99992922820282),
(1.,0.965925826289068,1.,0.965925826289068,1.,0.965925826289068,1.,0.965925826289068,
1.,0.965925826289068,1.,0.965925826289068,1.,0.965925826289068,1.,0.965925826289068,
1.,0.965925826289068,1.,0.965925826289068,1.,0.965925826289068,1.,0.965925826289068,
1.,0.965925826289068,1.,0.965925826289068,1.,0.965925826289068,1.,0.965925826289068,
1.,0.965925826289068,1.,0.965925826289068,1.,0.965925826289068,1.,0.965925826289068,
1.,0.965925826289068,1.,0.965925826289068,1.,0.965925826289068,1.,0.965925826289068,
1.,0.965925826289068,1.,0.965925826289068,1.,0.965925826289068,1.,0.965925826289068,
1.,0.965925826289068,1.,0.965925826289068,1.,0.965925826289068,1.,0.965925826289068,
1.,0.965925826289068,1.,0.965925826289068,1.,0.965925826289068,1.,0.965925826289068,
1.,0.965925826289068,1.,0.965925826289068,1.,0.965925826289068,1.,0.965925826289068,
1.,0.965925826289068,1.,0.965925826289068,1.,0.965925826289068,1.,0.965925826289068,
1.,0.965925826289068,1.,0.965925826289068,1.,0.965925826289068,1.,0.965925826289068,
1.,0.965925826289068,1.,0.965925826289068,1.,0.965925826289068,1.,0.965925826289068,
1.,0.965925826289068,1.,0.965925826289068,1.,0.965925826289068,1.,0.965925826289068,
1.,0.965925826289068,1.,0.965925826289068,1.,0.965925826289068,1.,0.965925826289068,
1.,0.965925826289068,1.,0.965925826289068,1.,0.965925826289068,1.,0.965925826289068,
1.,0.965925826289068,1.,0.965925826289068,1.,0.965925826289068,1.,0.965925826289068,
1.,0.965925826289068,1.,0.965925826289068,1.,0.965925826289068,1.,0.965925826289068,
1.,0.965925826289068,1.,0.965925826289068,1.,0.965925826289068,1.,0.965925826289068,
1.,0.965925826289068,1.,0.965925826289068,1.,0.965925826289068,1.,0.965925826289068,
1.,0.965925826289068,1.,0.965925826289068,1.,0.965925826289068,1.,0.965925826289068,
1.,0.965925826289068,1.,0.965925826289068,1.,0.965925826289068,1.,0.965925826289068,
1.,0.965925826289068,1.,0.965925826289068,1.,0.965925826289068,1.,0.965925826289068,
1.,0.965925826289068,1.,0.965925826289068,1.,0.965925826289068,1.,0.965925826289068,
1.),(0.333333333333333,0.321975275429689,0.333333333333333,0.321975275429689,
0.333333333333333,0.321975275429689,0.333333333333333,0.321975275429689,
0.333333333333333,0.321975275429689,0.333333333333333,0.321975275429689,
0.333333333333333,0.321975275429689,0.333333333333333,0.321975275429689,
0.333333333333333,0.321975275429689,0.333333333333333,0.321975275429689,
0.333333333333333,0.321975275429689,0.333333333333333,0.321975275429689,
0.333333333333333,0.321975275429689,0.333333333333333,0.321975275429689,
0.333333333333333,0.321975275429689,0.333333333333333,0.321975275429689,
0.333333333333333,0.321975275429689,0.333333333333333,0.321975275429689,
0.333333333333333,0.321975275429689,0.333333333333333,0.321975275429689,
0.333333333333333,0.321975275429689,0.333333333333333,0.321975275429689,
0.333333333333333,0.321975275429689,0.333333333333333,0.321975275429689,
0.333333333333333,0.321975275429689,0.333333333333333,0.321975275429689,
0.333333333333333,0.321975275429689,0.333333333333333,0.321975275429689,
0.333333333333333,0.321975275429689,0.333333333333333,0.321975275429689,
0.333333333333333,0.321975275429689,0.333333333333333,0.321975275429689,
0.333333333333333,0.321975275429689,0.333333333333333,0.321975275429689,
0.333333333333333,0.321975275429689,0.333333333333333,0.321975275429689,
0.333333333333333,0.321975275429689,0.333333333333333,0.321975275429689,
0.333333333333333,0.321975275429689,0.333333333333333,0.321975275429689,
0.333333333333333,0.321975275429689,0.333333333333333,0.321975275429689,
0.333333333333333,0.321975275429689,0.333333333333333,0.321975275429689,
0.333333333333333,0.321975275429689,0.333333333333333,0.321975275429689,
0.333333333333333,0.321975275429689,0.333333333333333,0.321975275429689,
0.333333333333333,0.321975275429689,0.333333333333333,0.321975275429689,
0.333333333333333,0.321975275429689,0.333333333333333,0.321975275429689,
0.333333333333333,0.321975275429689,0.333333333333333,0.321975275429689,
0.333333333333333,0.321975275429689,0.333333333333333,0.321975275429689,
0.333333333333333,0.321975275429689,0.333333333333333,0.321975275429689,
0.333333333333333,0.321975275429689,0.333333333333333,0.321975275429689,
0.333333333333333,0.321975275429689,0.333333333333333,0.321975275429689,
0.333333333333333,0.321975275429689,0.333333333333333,0.321975275429689,
0.333333333333333,0.321975275429689,0.333333333333333,0.321975275429689,
0.333333333333333,0.321975275429689,0.333333333333333,0.321975275429689,
0.333333333333333,0.321975275429689,0.333333333333333,0.321975275429689,
0.333333333333333,0.321975275429689,0.333333333333333,0.321975275429689,
0.333333333333333,0.321975275429689,0.333333333333333,0.321975275429689,
0.333333333333333,0.321975275429689,0.333333333333333,0.321975275429689,
0.333333333333333,0.321975275429689,0.333333333333333,0.321975275429689,
0.333333333333333,0.321975275429689,0.333333333333333,0.321975275429689,
0.333333333333333,0.321975275429689,0.333333333333333,0.321975275429689,
0.333333333333333,0.321975275429689,0.333333333333333,0.321975275429689,
0.333333333333333,0.321975275429689,0.333333333333333,0.321975275429689,
0.333333333333333,0.321975275429689,0.333333333333333,0.321975275429689,
0.333333333333333,0.321975275429689,0.333333333333333,0.321975275429689,
0.333333333333333,0.321975275429689,0.333333333333333,0.321975275429689,
0.333333333333333,0.321975275429689,0.333333333333333,0.321975275429689,
0.333333333333333,0.321975275429689,0.333333333333333,0.321975275429689,
0.333333333333333),(0.333333333333333,0.321975275429689,0.333333333333333,
0.321975275429689,0.333333333333333,0.321975275429689,0.333333333333333,
0.321975275429689,0.333333333333333,0.321975275429689,0.333333333333333,
0.321975275429689,0.333333333333333,0.321975275429689,0.333333333333333,
0.321975275429689,0.333333333333333,0.321975275429689,0.333333333333333,
0.321975275429689,0.333333333333333,0.321975275429689,0.333333333333333,
0.321975275429689,0.333333333333333,0.321975275429689,0.333333333333333,
0.321975275429689,0.333333333333333,0.321975275429689,0.333333333333333,
0.321975275429689,0.333333333333333,0.321975275429689,0.333333333333333,
0.321975275429689,0.333333333333333,0.321975275429689,0.333333333333333,
0.321975275429689,0.333333333333333,0.321975275429689,0.333333333333333,
0.321975275429689,0.333333333333333,0.321975275429689,0.333333333333333,
0.321975275429689,0.333333333333333,0.321975275429689,0.333333333333333,
0.321975275429689,0.333333333333333,0.321975275429689,0.333333333333333,
0.321975275429689,0.333333333333333,0.321975275429689,0.333333333333333,
0.321975275429689,0.333333333333333,0.321975275429689,0.333333333333333,
0.321975275429689,0.333333333333333,0.321975275429689,0.333333333333333,
0.321975275429689,0.333333333333333,0.321975275429689,0.333333333333333,
0.321975275429689,0.333333333333333,0.321975275429689,0.333333333333333,
0.321975275429689,0.333333333333333,0.321975275429689,0.333333333333333,
0.321975275429689,0.333333333333333,0.321975275429689,0.333333333333333,
0.321975275429689,0.333333333333333,0.321975275429689,0.333333333333333,
0.321975275429689,0.333333333333333,0.321975275429689,0.333333333333333,
0.321975275429689,0.333333333333333,0.321975275429689,0.333333333333333,
0.321975275429689,0.333333333333333,0.321975275429689,0.333333333333333,
0.321975275429689,0.333333333333333,0.321975275429689,0.333333333333333,
0.321975275429689,0.333333333333333,0.321975275429689,0.333333333333333,
0.321975275429689,0.333333333333333,0.321975275429689,0.333333333333333,
0.321975275429689,0.333333333333333,0.321975275429689,0.333333333333333,
0.321975275429689,0.333333333333333,0.321975275429689,0.333333333333333,
0.321975275429689,0.333333333333333,0.321975275429689,0.333333333333333,
0.321975275429689,0.333333333333333,0.321975275429689,0.333333333333333,
0.321975275429689,0.333333333333333,0.321975275429689,0.333333333333333,
0.321975275429689,0.333333333333333,0.321975275429689,0.333333333333333,
0.321975275429689,0.333333333333333,0.321975275429689,0.333333333333333,
0.321975275429689,0.333333333333333,0.321975275429689,0.333333333333333,
0.321975275429689,0.333333333333333,0.321975275429689,0.333333333333333,
0.321975275429689,0.333333333333333,0.321975275429689,0.333333333333333,
0.321975275429689,0.333333333333333,0.321975275429689,0.333333333333333,
0.321975275429689,0.333333333333333,0.321975275429689,0.333333333333333,
0.321975275429689,0.333333333333333,0.321975275429689,0.333333333333333,
0.321975275429689,0.333333333333333,0.321975275429689,0.333333333333333,
0.321975275429689,0.333333333333333,0.321975275429689,0.333333333333333,
0.321975275429689,0.333333333333333,0.321975275429689,0.333333333333333,
0.321975275429689,0.333333333333333,0.321975275429689,0.333333333333333,
0.321975275429689,0.333333333333333,0.321975275429689,0.333333333333333,
0.321975275429689,0.333333333333333,0.321975275429689,0.333333333333333,
0.321975275429689,0.333333333333333,0.321975275429689,0.333333333333333,
0.321975275429689,0.333333333333333),(1.,0.965925826289068,1.,0.965925826289068,
1.,0.965925826289068,1.,0.965925826289068,1.,0.965925826289068,1.,0.965925826289068,
1.,0.965925826289068,1.,0.965925826289068,1.,0.965925826289068,1.,0.965925826289068,
1.,0.965925826289068,1.,0.965925826289068,1.,0.965925826289068,1.,0.965925826289068,
1.,0.965925826289068,1.,0.965925826289068,1.,0.965925826289068,1.,0.965925826289068,
1.,0.965925826289068,1.,0.965925826289068,1.,0.965925826289068,1.,0.965925826289068,
1.,0.965925826289068,1.,0.965925826289068,1.,0.965925826289068,1.,0.965925826289068,
1.,0.965925826289068,1.,0.965925826289068,1.,0.965925826289068,1.,0.965925826289068,
1.,0.965925826289068,1.,0.965925826289068,1.,0.965925826289068,1.,0.965925826289068,
1.,0.965925826289068,1.,0.965925826289068,1.,0.965925826289068,1.,0.965925826289068,
1.,0.965925826289068,1.,0.965925826289068,1.,0.965925826289068,1.,0.965925826289068,
1.,0.965925826289068,1.,0.965925826289068,1.,0.965925826289068,1.,0.965925826289068,
1.,0.965925826289068,1.,0.965925826289068,1.,0.965925826289068,1.,0.965925826289068,
1.,0.965925826289068,1.,0.965925826289068,1.,0.965925826289068,1.,0.965925826289068,
1.,0.965925826289068,1.,0.965925826289068,1.,0.965925826289068,1.,0.965925826289068,
1.,0.965925826289068,1.,0.965925826289068,1.,0.965925826289068,1.,0.965925826289068,
1.,0.965925826289068,1.,0.965925826289068,1.,0.965925826289068,1.,0.965925826289068,
1.,0.965925826289068,1.,0.965925826289068,1.,0.965925826289068,1.,0.965925826289068,
1.,0.965925826289068,1.,0.965925826289068,1.,0.965925826289068,1.,0.965925826289068,
1.,0.965925826289068,1.,0.965925826289068,1.,0.965925826289068,1.,0.965925826289068,
1.,0.965925826289068,1.,0.965925826289068,1.,0.965925826289068,1.,0.965925826289068,
1.,0.965925826289068,1.,0.965925826289068,1.,0.965925826289068,1.,0.965925826289068,
1.,0.965925826289068,1.,0.965925826289068,1.,0.965925826289068,1.,0.965925826289068,
1.,0.965925826289068,1.,0.965925826289068,1.,0.965925826289068,1.,0.965925826289068,
1.,0.965925826289068,1.,0.965925826289068,1.),(0.333404105130514,0.322043635736359,
0.333404105130514,0.322043635736359,0.333404105130514,0.322043635736359,
0.333404105130514,0.322043635736359,0.333404105130514,0.322043635736359,
0.333404105130514,0.322043635736359,0.333404105130514,0.322043635736359,
0.333404105130514,0.322043635736359,0.333404105130514,0.322043635736359,
0.333404105130514,0.322043635736359,0.333404105130514,0.322043635736359,
0.333404105130514,0.322043635736359,0.333404105130514,0.322043635736359,
0.333404105130514,0.322043635736359,0.333404105130514,0.322043635736359,
0.333404105130514,0.322043635736359,0.333404105130514,0.322043635736359,
0.333404105130514,0.322043635736359,0.333404105130514,0.322043635736359,
0.333404105130514,0.322043635736359,0.333404105130514,0.322043635736359,
0.333404105130514,0.322043635736359,0.333404105130514,0.322043635736359,
0.333404105130514,0.322043635736359,0.333404105130514,0.322043635736359,
0.333404105130514,0.322043635736359,0.333404105130514,0.322043635736359,
0.333404105130514,0.322043635736359,0.333404105130514,0.322043635736359,
0.333404105130514,0.322043635736359,0.333404105130514,0.322043635736359,
0.333404105130514,0.322043635736359,0.333404105130514,0.322043635736359,
0.333404105130514,0.322043635736359,0.333404105130514,0.322043635736359,
0.333404105130514,0.322043635736359,0.333404105130514,0.322043635736359,
0.333404105130514,0.322043635736359,0.333404105130514,0.322043635736359,
0.333404105130514,0.322043635736359,0.333404105130514,0.322043635736359,
0.333404105130514,0.322043635736359,0.333404105130514,0.322043635736359,
0.333404105130514,0.322043635736359,0.333404105130514,0.322043635736359,
0.333404105130514,0.322043635736359,0.333404105130514,0.322043635736359,
0.333404105130514,0.322043635736359,0.333404105130514,0.322043635736359,
0.333404105130514,0.322043635736359,0.333404105130514,0.322043635736359,
0.333404105130514,0.322043635736359,0.333404105130514,0.322043635736359,
0.333404105130514,0.322043635736359,0.333404105130514,0.322043635736359,
0.333404105130514,0.322043635736359,0.333404105130514,0.322043635736359,
0.333404105130514,0.322043635736359,0.333404105130514,0.322043635736359,
0.333404105130514,0.322043635736359,0.333404105130514,0.322043635736359,
0.333404105130514,0.322043635736359,0.333404105130514,0.322043635736359,
0.333404105130514,0.322043635736359,0.333404105130514,0.322043635736359,
0.333404105130514,0.322043635736359,0.333404105130514,0.322043635736359,
0.333404105130514,0.322043635736359,0.333404105130514,0.322043635736359,
0.333404105130514,0.322043635736359,0.333404105130514,0.322043635736359,
0.333404105130514,0.322043635736359,0.333404105130514,0.322043635736359,
0.333404105130514,0.322043635736359,0.333404105130514,0.322043635736359,
0.333404105130514,0.322043635736359,0.333404105130514,0.322043635736359,
0.333404105130514,0.322043635736359,0.333404105130514,0.322043635736359,
0.333404105130514,0.322043635736359,0.333404105130514,0.322043635736359,
0.333404105130514,0.322043635736359,0.333404105130514,0.322043635736359,
0.333404105130514,0.322043635736359,0.333404105130514,0.322043635736359,
0.333404105130514,0.322043635736359,0.333404105130514,0.322043635736359,
0.333404105130514,0.322043635736359,0.333404105130514,0.322043635736359,
0.333404105130514,0.322043635736359,0.333404105130514,0.322043635736359,
0.333404105130514,0.322043635736359,0.333404105130514,0.322043635736359,
0.333404105130514,0.322043635736359,0.333404105130514,0.322043635736359,
0.333404105130514,0.322043635736359,0.333404105130514),(0.333333340846304,
0.321975282686662,0.333333340846304,0.321975282686662,0.333333340846304,
0.321975282686662,0.333333340846304,0.321975282686662,0.333333340846304,
0.321975282686662,0.333333340846304,0.321975282686662,0.333333340846304,
0.321975282686662,0.333333340846304,0.321975282686662,0.333333340846304,
0.321975282686662,0.333333340846304,0.321975282686662,0.333333340846304,
0.321975282686662,0.333333340846304,0.321975282686662,0.333333340846304,
0.321975282686662,0.333333340846304,0.321975282686662,0.333333340846304,
0.321975282686662,0.333333340846304,0.321975282686662,0.333333340846304,
0.321975282686662,0.333333340846304,0.321975282686662,0.333333340846304,
0.321975282686662,0.333333340846304,0.321975282686662,0.333333340846304,
0.321975282686662,0.333333340846304,0.321975282686662,0.333333340846304,
0.321975282686662,0.333333340846304,0.321975282686662,0.333333340846304,
0.321975282686662,0.333333340846304,0.321975282686662,0.333333340846304,
0.321975282686662,0.333333340846304,0.321975282686662,0.333333340846304,
0.321975282686662,0.333333340846304,0.321975282686662,0.333333340846304,
0.321975282686662,0.333333340846304,0.321975282686662,0.333333340846304,
0.321975282686662,0.333333340846304,0.321975282686662,0.333333340846304,
0.321975282686662,0.333333340846304,0.321975282686662,0.333333340846304,
0.321975282686662,0.333333340846304,0.321975282686662,0.333333340846304,
0.321975282686662,0.333333340846304,0.321975282686662,0.333333340846304,
0.321975282686662,0.333333340846304,0.321975282686662,0.333333340846304,
0.321975282686662,0.333333340846304,0.321975282686662,0.333333340846304,
0.321975282686662,0.333333340846304,0.321975282686662,0.333333340846304,
0.321975282686662,0.333333340846304,0.321975282686662,0.333333340846304,
0.321975282686662,0.333333340846304,0.321975282686662,0.333333340846304,
0.321975282686662,0.333333340846304,0.321975282686662,0.333333340846304,
0.321975282686662,0.333333340846304,0.321975282686662,0.333333340846304,
0.321975282686662,0.333333340846304,0.321975282686662,0.333333340846304,
0.321975282686662,0.333333340846304,0.321975282686662,0.333333340846304,
0.321975282686662,0.333333340846304,0.321975282686662,0.333333340846304,
0.321975282686662,0.333333340846304,0.321975282686662,0.333333340846304,
0.321975282686662,0.333333340846304,0.321975282686662,0.333333340846304,
0.321975282686662,0.333333340846304,0.321975282686662,0.333333340846304,
0.321975282686662,0.333333340846304,0.321975282686662,0.333333340846304,
0.321975282686662,0.333333340846304,0.321975282686662,0.333333340846304,
0.321975282686662,0.333333340846304,0.321975282686662,0.333333340846304,
0.321975282686662,0.333333340846304,0.321975282686662,0.333333340846304,
0.321975282686662,0.333333340846304,0.321975282686662,0.333333340846304,
0.321975282686662,0.333333340846304,0.321975282686662,0.333333340846304,
0.321975282686662,0.333333340846304,0.321975282686662,0.333333340846304,
0.321975282686662,0.333333340846304,0.321975282686662,0.333333340846304,
0.321975282686662,0.333333340846304,0.321975282686662,0.333333340846304,
0.321975282686662,0.333333340846304,0.321975282686662,0.333333340846304,
0.321975282686662,0.333333340846304,0.321975282686662,0.333333340846304,
0.321975282686662,0.333333340846304,0.321975282686662,0.333333340846304,
0.321975282686662,0.333333340846304,0.321975282686662,0.333333340846304,
0.321975282686662,0.333333340846304,0.321975282686662,0.333333340846304,
0.321975282686662,0.333333340846304,0.321975282686662,0.333333340846304),
(0.999787707147372,0.965720767139978,0.999787707147372,0.965720767139978,
0.999787707147372,0.965720767139978,0.999787707147372,0.965720767139978,
0.999787707147372,0.965720767139978,0.999787707147372,0.965720767139978,
0.999787707147372,0.965720767139978,0.999787707147372,0.965720767139978,
0.999787707147372,0.965720767139978,0.999787707147372,0.965720767139978,
0.999787707147372,0.965720767139978,0.999787707147372,0.965720767139978,
0.999787707147372,0.965720767139978,0.999787707147372,0.965720767139978,
0.999787707147372,0.965720767139978,0.999787707147372,0.965720767139978,
0.999787707147372,0.965720767139978,0.999787707147372,0.965720767139978,
0.999787707147372,0.965720767139978,0.999787707147372,0.965720767139978,
0.999787707147372,0.965720767139978,0.999787707147372,0.965720767139978,
0.999787707147372,0.965720767139978,0.999787707147372,0.965720767139978,
0.999787707147372,0.965720767139978,0.999787707147372,0.965720767139978,
0.999787707147372,0.965720767139978,0.999787707147372,0.965720767139978,
0.999787707147372,0.965720767139978,0.999787707147372,0.965720767139978,
0.999787707147372,0.965720767139978,0.999787707147372,0.965720767139978,
0.999787707147372,0.965720767139978,0.999787707147372,0.965720767139978,
0.999787707147372,0.965720767139978,0.999787707147372,0.965720767139978,
0.999787707147372,0.965720767139978,0.999787707147372,0.965720767139978,
0.999787707147372,0.965720767139978,0.999787707147372,0.965720767139978,
0.999787707147372,0.965720767139978,0.999787707147372,0.965720767139978,
0.999787707147372,0.965720767139978,0.999787707147372,0.965720767139978,
0.999787707147372,0.965720767139978,0.999787707147372,0.965720767139978,
0.999787707147372,0.965720767139978,0.999787707147372,0.965720767139978,
0.999787707147372,0.965720767139978,0.999787707147372,0.965720767139978,
0.999787707147372,0.965720767139978,0.999787707147372,0.965720767139978,
0.999787707147372,0.965720767139978,0.999787707147372,0.965720767139978,
0.999787707147372,0.965720767139978,0.999787707147372,0.965720767139978,
0.999787707147372,0.965720767139978,0.999787707147372,0.965720767139978,
0.999787707147372,0.965720767139978,0.999787707147372,0.965720767139978,
0.999787707147372,0.965720767139978,0.999787707147372,0.965720767139978,
0.999787707147372,0.965720767139978,0.999787707147372,0.965720767139978,
0.999787707147372,0.965720767139978,0.999787707147372,0.965720767139978,
0.999787707147372,0.965720767139978,0.999787707147372,0.965720767139978,
0.999787707147372,0.965720767139978,0.999787707147372,0.965720767139978,
0.999787707147372,0.965720767139978,0.999787707147372,0.965720767139978,
0.999787707147372,0.965720767139978,0.999787707147372,0.965720767139978,
0.999787707147372,0.965720767139978,0.999787707147372,0.965720767139978,
0.999787707147372,0.965720767139978,0.999787707147372,0.965720767139978,
0.999787707147372,0.965720767139978,0.999787707147372,0.965720767139978,
0.999787707147372,0.965720767139978,0.999787707147372,0.965720767139978,
0.999787707147372,0.965720767139978,0.999787707147372,0.965720767139978,
0.999787707147372,0.965720767139978,0.999787707147372,0.965720767139978,
0.999787707147372,0.965720767139978,0.999787707147372,0.965720767139978,
0.999787707147372,0.965720767139978,0.999787707147372,0.965720767139978,
0.999787707147372,0.965720767139978,0.999787707147372,0.965720767139978,
0.999787707147372,0.965720767139978,0.999787707147372,0.965720767139978,
0.999787707147372,0.965720767139978,0.999787707147372,0.965720767139978,
0.999787707147372)))
REPRESENTATION_ITEM('')
SURFACE()
);
#18=(
BOUNDED_SURFACE()
B_SPLINE_SURFACE(3,2,((#9944,#9945,#9946,#9947,#9948,#9949,#9950,#9951,
#9952,#9953,#9954,#9955,#9956,#9957,#9958,#9959,#9960,#9961,#9962,#9963,
#9964,#9965,#9966,#9967,#9968,#9969,#9970,#9971,#9972,#9973,#9974,#9975,
#9976,#9977,#9978,#9979,#9980,#9981,#9982,#9983,#9984,#9985,#9986,#9987,
#9988,#9989,#9990,#9991,#9992,#9993,#9994,#9995,#9996,#9997,#9998,#9999,
#10000,#10001,#10002,#10003,#10004,#10005,#10006,#10007,#10008,#10009,#10010,
#10011,#10012,#10013,#10014,#10015,#10016,#10017,#10018,#10019,#10020,#10021,
#10022,#10023,#10024,#10025,#10026,#10027,#10028,#10029,#10030,#10031,#10032,
#10033,#10034,#10035,#10036,#10037,#10038,#10039,#10040,#10041,#10042,#10043,
#10044,#10045,#10046,#10047,#10048,#10049,#10050,#10051,#10052,#10053,#10054,
#10055,#10056,#10057,#10058,#10059,#10060,#10061,#10062,#10063,#10064,#10065,
#10066,#10067,#10068,#10069,#10070,#10071,#10072,#10073,#10074,#10075,#10076,
#10077,#10078,#10079,#10080,#10081,#10082,#10083,#10084,#10085,#10086,#10087,
#10088,#10089,#10090,#10091,#10092,#10093,#10094,#10095,#10096,#10097,#10098,
#10099,#10100,#10101,#10102,#10103,#10104,#10105,#10106,#10107,#10108,#10109,
#10110,#10111,#10112,#10113,#10114,#10115,#10116,#10117,#10118,#10119,#10120,
#10121,#10122,#10123,#10124,#10125,#10126,#10127,#10128,#10129,#10130,#10131,
#10132,#10133,#10134,#10135,#10136),(#10137,#10138,#10139,#10140,#10141,
#10142,#10143,#10144,#10145,#10146,#10147,#10148,#10149,#10150,#10151,#10152,
#10153,#10154,#10155,#10156,#10157,#10158,#10159,#10160,#10161,#10162,#10163,
#10164,#10165,#10166,#10167,#10168,#10169,#10170,#10171,#10172,#10173,#10174,
#10175,#10176,#10177,#10178,#10179,#10180,#10181,#10182,#10183,#10184,#10185,
#10186,#10187,#10188,#10189,#10190,#10191,#10192,#10193,#10194,#10195,#10196,
#10197,#10198,#10199,#10200,#10201,#10202,#10203,#10204,#10205,#10206,#10207,
#10208,#10209,#10210,#10211,#10212,#10213,#10214,#10215,#10216,#10217,#10218,
#10219,#10220,#10221,#10222,#10223,#10224,#10225,#10226,#10227,#10228,#10229,
#10230,#10231,#10232,#10233,#10234,#10235,#10236,#10237,#10238,#10239,#10240,
#10241,#10242,#10243,#10244,#10245,#10246,#10247,#10248,#10249,#10250,#10251,
#10252,#10253,#10254,#10255,#10256,#10257,#10258,#10259,#10260,#10261,#10262,
#10263,#10264,#10265,#10266,#10267,#10268,#10269,#10270,#10271,#10272,#10273,
#10274,#10275,#10276,#10277,#10278,#10279,#10280,#10281,#10282,#10283,#10284,
#10285,#10286,#10287,#10288,#10289,#10290,#10291,#10292,#10293,#10294,#10295,
#10296,#10297,#10298,#10299,#10300,#10301,#10302,#10303,#10304,#10305,#10306,
#10307,#10308,#10309,#10310,#10311,#10312,#10313,#10314,#10315,#10316,#10317,
#10318,#10319,#10320,#10321,#10322,#10323,#10324,#10325,#10326,#10327,#10328,
#10329),(#10330,#10331,#10332,#10333,#10334,#10335,#10336,#10337,#10338,
#10339,#10340,#10341,#10342,#10343,#10344,#10345,#10346,#10347,#10348,#10349,
#10350,#10351,#10352,#10353,#10354,#10355,#10356,#10357,#10358,#10359,#10360,
#10361,#10362,#10363,#10364,#10365,#10366,#10367,#10368,#10369,#10370,#10371,
#10372,#10373,#10374,#10375,#10376,#10377,#10378,#10379,#10380,#10381,#10382,
#10383,#10384,#10385,#10386,#10387,#10388,#10389,#10390,#10391,#10392,#10393,
#10394,#10395,#10396,#10397,#10398,#10399,#10400,#10401,#10402,#10403,#10404,
#10405,#10406,#10407,#10408,#10409,#10410,#10411,#10412,#10413,#10414,#10415,
#10416,#10417,#10418,#10419,#10420,#10421,#10422,#10423,#10424,#10425,#10426,
#10427,#10428,#10429,#10430,#10431,#10432,#10433,#10434,#10435,#10436,#10437,
#10438,#10439,#10440,#10441,#10442,#10443,#10444,#10445,#10446,#10447,#10448,
#10449,#10450,#10451,#10452,#10453,#10454,#10455,#10456,#10457,#10458,#10459,
#10460,#10461,#10462,#10463,#10464,#10465,#10466,#10467,#10468,#10469,#10470,
#10471,#10472,#10473,#10474,#10475,#10476,#10477,#10478,#10479,#10480,#10481,
#10482,#10483,#10484,#10485,#10486,#10487,#10488,#10489,#10490,#10491,#10492,
#10493,#10494,#10495,#10496,#10497,#10498,#10499,#10500,#10501,#10502,#10503,
#10504,#10505,#10506,#10507,#10508,#10509,#10510,#10511,#10512,#10513,#10514,
#10515,#10516,#10517,#10518,#10519,#10520,#10521,#10522),(#10523,#10524,
#10525,#10526,#10527,#10528,#10529,#10530,#10531,#10532,#10533,#10534,#10535,
#10536,#10537,#10538,#10539,#10540,#10541,#10542,#10543,#10544,#10545,#10546,
#10547,#10548,#10549,#10550,#10551,#10552,#10553,#10554,#10555,#10556,#10557,
#10558,#10559,#10560,#10561,#10562,#10563,#10564,#10565,#10566,#10567,#10568,
#10569,#10570,#10571,#10572,#10573,#10574,#10575,#10576,#10577,#10578,#10579,
#10580,#10581,#10582,#10583,#10584,#10585,#10586,#10587,#10588,#10589,#10590,
#10591,#10592,#10593,#10594,#10595,#10596,#10597,#10598,#10599,#10600,#10601,
#10602,#10603,#10604,#10605,#10606,#10607,#10608,#10609,#10610,#10611,#10612,
#10613,#10614,#10615,#10616,#10617,#10618,#10619,#10620,#10621,#10622,#10623,
#10624,#10625,#10626,#10627,#10628,#10629,#10630,#10631,#10632,#10633,#10634,
#10635,#10636,#10637,#10638,#10639,#10640,#10641,#10642,#10643,#10644,#10645,
#10646,#10647,#10648,#10649,#10650,#10651,#10652,#10653,#10654,#10655,#10656,
#10657,#10658,#10659,#10660,#10661,#10662,#10663,#10664,#10665,#10666,#10667,
#10668,#10669,#10670,#10671,#10672,#10673,#10674,#10675,#10676,#10677,#10678,
#10679,#10680,#10681,#10682,#10683,#10684,#10685,#10686,#10687,#10688,#10689,
#10690,#10691,#10692,#10693,#10694,#10695,#10696,#10697,#10698,#10699,#10700,
#10701,#10702,#10703,#10704,#10705,#10706,#10707,#10708,#10709,#10710,#10711,
#10712,#10713,#10714,#10715),(#10716,#10717,#10718,#10719,#10720,#10721,
#10722,#10723,#10724,#10725,#10726,#10727,#10728,#10729,#10730,#10731,#10732,
#10733,#10734,#10735,#10736,#10737,#10738,#10739,#10740,#10741,#10742,#10743,
#10744,#10745,#10746,#10747,#10748,#10749,#10750,#10751,#10752,#10753,#10754,
#10755,#10756,#10757,#10758,#10759,#10760,#10761,#10762,#10763,#10764,#10765,
#10766,#10767,#10768,#10769,#10770,#10771,#10772,#10773,#10774,#10775,#10776,
#10777,#10778,#10779,#10780,#10781,#10782,#10783,#10784,#10785,#10786,#10787,
#10788,#10789,#10790,#10791,#10792,#10793,#10794,#10795,#10796,#10797,#10798,
#10799,#10800,#10801,#10802,#10803,#10804,#10805,#10806,#10807,#10808,#10809,
#10810,#10811,#10812,#10813,#10814,#10815,#10816,#10817,#10818,#10819,#10820,
#10821,#10822,#10823,#10824,#10825,#10826,#10827,#10828,#10829,#10830,#10831,
#10832,#10833,#10834,#10835,#10836,#10837,#10838,#10839,#10840,#10841,#10842,
#10843,#10844,#10845,#10846,#10847,#10848,#10849,#10850,#10851,#10852,#10853,
#10854,#10855,#10856,#10857,#10858,#10859,#10860,#10861,#10862,#10863,#10864,
#10865,#10866,#10867,#10868,#10869,#10870,#10871,#10872,#10873,#10874,#10875,
#10876,#10877,#10878,#10879,#10880,#10881,#10882,#10883,#10884,#10885,#10886,
#10887,#10888,#10889,#10890,#10891,#10892,#10893,#10894,#10895,#10896,#10897,
#10898,#10899,#10900,#10901,#10902,#10903,#10904,#10905,#10906,#10907,#10908),
(#10909,#10910,#10911,#10912,#10913,#10914,#10915,#10916,#10917,#10918,
#10919,#10920,#10921,#10922,#10923,#10924,#10925,#10926,#10927,#10928,#10929,
#10930,#10931,#10932,#10933,#10934,#10935,#10936,#10937,#10938,#10939,#10940,
#10941,#10942,#10943,#10944,#10945,#10946,#10947,#10948,#10949,#10950,#10951,
#10952,#10953,#10954,#10955,#10956,#10957,#10958,#10959,#10960,#10961,#10962,
#10963,#10964,#10965,#10966,#10967,#10968,#10969,#10970,#10971,#10972,#10973,
#10974,#10975,#10976,#10977,#10978,#10979,#10980,#10981,#10982,#10983,#10984,
#10985,#10986,#10987,#10988,#10989,#10990,#10991,#10992,#10993,#10994,#10995,
#10996,#10997,#10998,#10999,#11000,#11001,#11002,#11003,#11004,#11005,#11006,
#11007,#11008,#11009,#11010,#11011,#11012,#11013,#11014,#11015,#11016,#11017,
#11018,#11019,#11020,#11021,#11022,#11023,#11024,#11025,#11026,#11027,#11028,
#11029,#11030,#11031,#11032,#11033,#11034,#11035,#11036,#11037,#11038,#11039,
#11040,#11041,#11042,#11043,#11044,#11045,#11046,#11047,#11048,#11049,#11050,
#11051,#11052,#11053,#11054,#11055,#11056,#11057,#11058,#11059,#11060,#11061,
#11062,#11063,#11064,#11065,#11066,#11067,#11068,#11069,#11070,#11071,#11072,
#11073,#11074,#11075,#11076,#11077,#11078,#11079,#11080,#11081,#11082,#11083,
#11084,#11085,#11086,#11087,#11088,#11089,#11090,#11091,#11092,#11093,#11094,
#11095,#11096,#11097,#11098,#11099,#11100,#11101),(#11102,#11103,#11104,
#11105,#11106,#11107,#11108,#11109,#11110,#11111,#11112,#11113,#11114,#11115,
#11116,#11117,#11118,#11119,#11120,#11121,#11122,#11123,#11124,#11125,#11126,
#11127,#11128,#11129,#11130,#11131,#11132,#11133,#11134,#11135,#11136,#11137,
#11138,#11139,#11140,#11141,#11142,#11143,#11144,#11145,#11146,#11147,#11148,
#11149,#11150,#11151,#11152,#11153,#11154,#11155,#11156,#11157,#11158,#11159,
#11160,#11161,#11162,#11163,#11164,#11165,#11166,#11167,#11168,#11169,#11170,
#11171,#11172,#11173,#11174,#11175,#11176,#11177,#11178,#11179,#11180,#11181,
#11182,#11183,#11184,#11185,#11186,#11187,#11188,#11189,#11190,#11191,#11192,
#11193,#11194,#11195,#11196,#11197,#11198,#11199,#11200,#11201,#11202,#11203,
#11204,#11205,#11206,#11207,#11208,#11209,#11210,#11211,#11212,#11213,#11214,
#11215,#11216,#11217,#11218,#11219,#11220,#11221,#11222,#11223,#11224,#11225,
#11226,#11227,#11228,#11229,#11230,#11231,#11232,#11233,#11234,#11235,#11236,
#11237,#11238,#11239,#11240,#11241,#11242,#11243,#11244,#11245,#11246,#11247,
#11248,#11249,#11250,#11251,#11252,#11253,#11254,#11255,#11256,#11257,#11258,
#11259,#11260,#11261,#11262,#11263,#11264,#11265,#11266,#11267,#11268,#11269,
#11270,#11271,#11272,#11273,#11274,#11275,#11276,#11277,#11278,#11279,#11280,
#11281,#11282,#11283,#11284,#11285,#11286,#11287,#11288,#11289,#11290,#11291,
#11292,#11293,#11294)),.UNSPECIFIED.,.T.,.F.,.F.)
B_SPLINE_SURFACE_WITH_KNOTS((4,3,4),(3,2,2,2,2,2,2,2,2,2,2,2,2,2,2,2,2,
2,2,2,2,2,2,2,2,2,2,2,2,2,2,2,2,2,2,2,2,2,2,2,2,2,2,2,2,2,2,2,2,2,2,2,2,
2,2,2,2,2,2,2,2,2,2,2,2,2,2,2,2,2,2,2,2,2,2,2,2,2,2,2,2,2,2,2,2,2,2,2,2,
2,2,2,2,2,2,2,3),(0.,0.5,1.),(0.,0.0104166666666667,0.0208333333333333,
0.03125,0.0416666666666667,0.0520833333333333,0.0625,0.0729166666666667,
0.0833333333333333,0.09375,0.104166666666667,0.114583333333333,0.125,0.135416666666667,
0.145833333333333,0.15625,0.166666666666667,0.177083333333333,0.1875,0.197916666666667,
0.208333333333333,0.21875,0.229166666666667,0.239583333333333,0.25,0.260416666666667,
0.270833333333333,0.28125,0.291666666666667,0.302083333333333,0.3125,0.322916666666667,
0.333333333333333,0.34375,0.354166666666667,0.364583333333333,0.375,0.385416666666667,
0.395833333333333,0.40625,0.416666666666667,0.427083333333333,0.4375,0.447916666666667,
0.458333333333333,0.46875,0.479166666666667,0.489583333333333,0.5,0.510416666666667,
0.520833333333333,0.53125,0.541666666666667,0.552083333333333,0.5625,0.572916666666667,
0.583333333333333,0.59375,0.604166666666667,0.614583333333333,0.625,0.635416666666667,
0.645833333333333,0.65625,0.666666666666667,0.677083333333333,0.6875,0.697916666666667,
0.708333333333333,0.71875,0.729166666666667,0.739583333333333,0.75,0.760416666666667,
0.770833333333333,0.78125,0.791666666666667,0.802083333333333,0.8125,0.822916666666667,
0.833333333333333,0.84375,0.854166666666667,0.864583333333333,0.875,0.885416666666667,
0.895833333333333,0.90625,0.916666666666667,0.927083333333333,0.9375,0.947916666666667,
0.958333333333333,0.96875,0.979166666666667,0.989583333333333,1.),
 .UNSPECIFIED.)
GEOMETRIC_REPRESENTATION_ITEM()
RATIONAL_B_SPLINE_SURFACE(((1.,0.965925826289068,1.,0.965925826289068,1.,
0.965925826289068,1.,0.965925826289068,1.,0.965925826289068,1.,0.965925826289068,
1.,0.965925826289068,1.,0.965925826289068,1.,0.965925826289068,1.,0.965925826289068,
1.,0.965925826289068,1.,0.965925826289068,1.,0.965925826289068,1.,0.965925826289068,
1.,0.965925826289068,1.,0.965925826289068,1.,0.965925826289068,1.,0.965925826289068,
1.,0.965925826289068,1.,0.965925826289068,1.,0.965925826289068,1.,0.965925826289068,
1.,0.965925826289068,1.,0.965925826289068,1.,0.965925826289068,1.,0.965925826289068,
1.,0.965925826289068,1.,0.965925826289068,1.,0.965925826289068,1.,0.965925826289068,
1.,0.965925826289068,1.,0.965925826289068,1.,0.965925826289068,1.,0.965925826289068,
1.,0.965925826289068,1.,0.965925826289068,1.,0.965925826289068,1.,0.965925826289068,
1.,0.965925826289068,1.,0.965925826289068,1.,0.965925826289068,1.,0.965925826289068,
1.,0.965925826289068,1.,0.965925826289068,1.,0.965925826289068,1.,0.965925826289068,
1.,0.965925826289068,1.,0.965925826289068,1.,0.965925826289068,1.,0.965925826289068,
1.,0.965925826289068,1.,0.965925826289068,1.,0.965925826289068,1.,0.965925826289068,
1.,0.965925826289068,1.,0.965925826289068,1.,0.965925826289068,1.,0.965925826289068,
1.,0.965925826289068,1.,0.965925826289068,1.,0.965925826289068,1.,0.965925826289068,
1.,0.965925826289068,1.,0.965925826289068,1.,0.965925826289068,1.,0.965925826289068,
1.,0.965925826289068,1.,0.965925826289068,1.,0.965925826289068,1.,0.965925826289068,
1.,0.965925826289068,1.,0.965925826289068,1.,0.965925826289068,1.,0.965925826289068,
1.,0.965925826289068,1.,0.965925826289068,1.,0.965925826289068,1.,0.965925826289068,
1.,0.965925826289068,1.,0.965925826289068,1.,0.965925826289068,1.,0.965925826289068,
1.,0.965925826289068,1.,0.965925826289068,1.,0.965925826289068,1.,0.965925826289068,
1.,0.965925826289068,1.,0.965925826289068,1.,0.965925826289068,1.,0.965925826289068,
1.,0.965925826289068,1.,0.965925826289068,1.,0.965925826289068,1.,0.965925826289068,
1.,0.965925826289068,1.,0.965925826289068,1.),(0.333333333333333,0.321975275429689,
0.333333333333333,0.321975275429689,0.333333333333333,0.321975275429689,
0.333333333333333,0.321975275429689,0.333333333333333,0.321975275429689,
0.333333333333333,0.321975275429689,0.333333333333333,0.321975275429689,
0.333333333333333,0.321975275429689,0.333333333333333,0.321975275429689,
0.333333333333333,0.321975275429689,0.333333333333333,0.321975275429689,
0.333333333333333,0.321975275429689,0.333333333333333,0.321975275429689,
0.333333333333333,0.321975275429689,0.333333333333333,0.321975275429689,
0.333333333333333,0.321975275429689,0.333333333333333,0.321975275429689,
0.333333333333333,0.321975275429689,0.333333333333333,0.321975275429689,
0.333333333333333,0.321975275429689,0.333333333333333,0.321975275429689,
0.333333333333333,0.321975275429689,0.333333333333333,0.321975275429689,
0.333333333333333,0.321975275429689,0.333333333333333,0.321975275429689,
0.333333333333333,0.321975275429689,0.333333333333333,0.321975275429689,
0.333333333333333,0.321975275429689,0.333333333333333,0.321975275429689,
0.333333333333333,0.321975275429689,0.333333333333333,0.321975275429689,
0.333333333333333,0.321975275429689,0.333333333333333,0.321975275429689,
0.333333333333333,0.321975275429689,0.333333333333333,0.321975275429689,
0.333333333333333,0.321975275429689,0.333333333333333,0.321975275429689,
0.333333333333333,0.321975275429689,0.333333333333333,0.321975275429689,
0.333333333333333,0.321975275429689,0.333333333333333,0.321975275429689,
0.333333333333333,0.321975275429689,0.333333333333333,0.321975275429689,
0.333333333333333,0.321975275429689,0.333333333333333,0.321975275429689,
0.333333333333333,0.321975275429689,0.333333333333333,0.321975275429689,
0.333333333333333,0.321975275429689,0.333333333333333,0.321975275429689,
0.333333333333333,0.321975275429689,0.333333333333333,0.321975275429689,
0.333333333333333,0.321975275429689,0.333333333333333,0.321975275429689,
0.333333333333333,0.321975275429689,0.333333333333333,0.321975275429689,
0.333333333333333,0.321975275429689,0.333333333333333,0.321975275429689,
0.333333333333333,0.321975275429689,0.333333333333333,0.321975275429689,
0.333333333333333,0.321975275429689,0.333333333333333,0.321975275429689,
0.333333333333333,0.321975275429689,0.333333333333333,0.321975275429689,
0.333333333333333,0.321975275429689,0.333333333333333,0.321975275429689,
0.333333333333333,0.321975275429689,0.333333333333333,0.321975275429689,
0.333333333333333,0.321975275429689,0.333333333333333,0.321975275429689,
0.333333333333333,0.321975275429689,0.333333333333333,0.321975275429689,
0.333333333333333,0.321975275429689,0.333333333333333,0.321975275429689,
0.333333333333333,0.321975275429689,0.333333333333333,0.321975275429689,
0.333333333333333,0.321975275429689,0.333333333333333,0.321975275429689,
0.333333333333333,0.321975275429689,0.333333333333333,0.321975275429689,
0.333333333333333,0.321975275429689,0.333333333333333,0.321975275429689,
0.333333333333333,0.321975275429689,0.333333333333333,0.321975275429689,
0.333333333333333,0.321975275429689,0.333333333333333,0.321975275429689,
0.333333333333333,0.321975275429689,0.333333333333333,0.321975275429689,
0.333333333333333,0.321975275429689,0.333333333333333,0.321975275429689,
0.333333333333333,0.321975275429689,0.333333333333333,0.321975275429689,
0.333333333333333,0.321975275429689,0.333333333333333,0.321975275429689,
0.333333333333333,0.321975275429689,0.333333333333333,0.321975275429689,
0.333333333333333,0.321975275429689,0.333333333333333),(0.333333333333333,
0.321975275429689,0.333333333333333,0.321975275429689,0.333333333333333,
0.321975275429689,0.333333333333333,0.321975275429689,0.333333333333333,
0.321975275429689,0.333333333333333,0.321975275429689,0.333333333333333,
0.321975275429689,0.333333333333333,0.321975275429689,0.333333333333333,
0.321975275429689,0.333333333333333,0.321975275429689,0.333333333333333,
0.321975275429689,0.333333333333333,0.321975275429689,0.333333333333333,
0.321975275429689,0.333333333333333,0.321975275429689,0.333333333333333,
0.321975275429689,0.333333333333333,0.321975275429689,0.333333333333333,
0.321975275429689,0.333333333333333,0.321975275429689,0.333333333333333,
0.321975275429689,0.333333333333333,0.321975275429689,0.333333333333333,
0.321975275429689,0.333333333333333,0.321975275429689,0.333333333333333,
0.321975275429689,0.333333333333333,0.321975275429689,0.333333333333333,
0.321975275429689,0.333333333333333,0.321975275429689,0.333333333333333,
0.321975275429689,0.333333333333333,0.321975275429689,0.333333333333333,
0.321975275429689,0.333333333333333,0.321975275429689,0.333333333333333,
0.321975275429689,0.333333333333333,0.321975275429689,0.333333333333333,
0.321975275429689,0.333333333333333,0.321975275429689,0.333333333333333,
0.321975275429689,0.333333333333333,0.321975275429689,0.333333333333333,
0.321975275429689,0.333333333333333,0.321975275429689,0.333333333333333,
0.321975275429689,0.333333333333333,0.321975275429689,0.333333333333333,
0.321975275429689,0.333333333333333,0.321975275429689,0.333333333333333,
0.321975275429689,0.333333333333333,0.321975275429689,0.333333333333333,
0.321975275429689,0.333333333333333,0.321975275429689,0.333333333333333,
0.321975275429689,0.333333333333333,0.321975275429689,0.333333333333333,
0.321975275429689,0.333333333333333,0.321975275429689,0.333333333333333,
0.321975275429689,0.333333333333333,0.321975275429689,0.333333333333333,
0.321975275429689,0.333333333333333,0.321975275429689,0.333333333333333,
0.321975275429689,0.333333333333333,0.321975275429689,0.333333333333333,
0.321975275429689,0.333333333333333,0.321975275429689,0.333333333333333,
0.321975275429689,0.333333333333333,0.321975275429689,0.333333333333333,
0.321975275429689,0.333333333333333,0.321975275429689,0.333333333333333,
0.321975275429689,0.333333333333333,0.321975275429689,0.333333333333333,
0.321975275429689,0.333333333333333,0.321975275429689,0.333333333333333,
0.321975275429689,0.333333333333333,0.321975275429689,0.333333333333333,
0.321975275429689,0.333333333333333,0.321975275429689,0.333333333333333,
0.321975275429689,0.333333333333333,0.321975275429689,0.333333333333333,
0.321975275429689,0.333333333333333,0.321975275429689,0.333333333333333,
0.321975275429689,0.333333333333333,0.321975275429689,0.333333333333333,
0.321975275429689,0.333333333333333,0.321975275429689,0.333333333333333,
0.321975275429689,0.333333333333333,0.321975275429689,0.333333333333333,
0.321975275429689,0.333333333333333,0.321975275429689,0.333333333333333,
0.321975275429689,0.333333333333333,0.321975275429689,0.333333333333333,
0.321975275429689,0.333333333333333,0.321975275429689,0.333333333333333,
0.321975275429689,0.333333333333333,0.321975275429689,0.333333333333333,
0.321975275429689,0.333333333333333,0.321975275429689,0.333333333333333,
0.321975275429689,0.333333333333333,0.321975275429689,0.333333333333333,
0.321975275429689,0.333333333333333,0.321975275429689,0.333333333333333,
0.321975275429689,0.333333333333333,0.321975275429689,0.333333333333333),
(1.,0.965925826289068,1.,0.965925826289068,1.,0.965925826289068,1.,0.965925826289068,
1.,0.965925826289068,1.,0.965925826289068,1.,0.965925826289068,1.,0.965925826289068,
1.,0.965925826289068,1.,0.965925826289068,1.,0.965925826289068,1.,0.965925826289068,
1.,0.965925826289068,1.,0.965925826289068,1.,0.965925826289068,1.,0.965925826289068,
1.,0.965925826289068,1.,0.965925826289068,1.,0.965925826289068,1.,0.965925826289068,
1.,0.965925826289068,1.,0.965925826289068,1.,0.965925826289068,1.,0.965925826289068,
1.,0.965925826289068,1.,0.965925826289068,1.,0.965925826289068,1.,0.965925826289068,
1.,0.965925826289068,1.,0.965925826289068,1.,0.965925826289068,1.,0.965925826289068,
1.,0.965925826289068,1.,0.965925826289068,1.,0.965925826289068,1.,0.965925826289068,
1.,0.965925826289068,1.,0.965925826289068,1.,0.965925826289068,1.,0.965925826289068,
1.,0.965925826289068,1.,0.965925826289068,1.,0.965925826289068,1.,0.965925826289068,
1.,0.965925826289068,1.,0.965925826289068,1.,0.965925826289068,1.,0.965925826289068,
1.,0.965925826289068,1.,0.965925826289068,1.,0.965925826289068,1.,0.965925826289068,
1.,0.965925826289068,1.,0.965925826289068,1.,0.965925826289068,1.,0.965925826289068,
1.,0.965925826289068,1.,0.965925826289068,1.,0.965925826289068,1.,0.965925826289068,
1.,0.965925826289068,1.,0.965925826289068,1.,0.965925826289068,1.,0.965925826289068,
1.,0.965925826289068,1.,0.965925826289068,1.,0.965925826289068,1.,0.965925826289068,
1.,0.965925826289068,1.,0.965925826289068,1.,0.965925826289068,1.,0.965925826289068,
1.,0.965925826289068,1.,0.965925826289068,1.,0.965925826289068,1.,0.965925826289068,
1.,0.965925826289068,1.,0.965925826289068,1.,0.965925826289068,1.,0.965925826289068,
1.,0.965925826289068,1.,0.965925826289068,1.,0.965925826289068,1.,0.965925826289068,
1.,0.965925826289068,1.,0.965925826289068,1.,0.965925826289068,1.,0.965925826289068,
1.,0.965925826289068,1.,0.965925826289068,1.,0.965925826289068,1.,0.965925826289068,
1.,0.965925826289068,1.,0.965925826289068,1.,0.965925826289068,1.,0.965925826289068,
1.),(0.333333333333333,0.321975275429689,0.333333333333333,0.321975275429689,
0.333333333333333,0.321975275429689,0.333333333333333,0.321975275429689,
0.333333333333333,0.321975275429689,0.333333333333333,0.321975275429689,
0.333333333333333,0.321975275429689,0.333333333333333,0.321975275429689,
0.333333333333333,0.321975275429689,0.333333333333333,0.321975275429689,
0.333333333333333,0.321975275429689,0.333333333333333,0.321975275429689,
0.333333333333333,0.321975275429689,0.333333333333333,0.321975275429689,
0.333333333333333,0.321975275429689,0.333333333333333,0.321975275429689,
0.333333333333333,0.321975275429689,0.333333333333333,0.321975275429689,
0.333333333333333,0.321975275429689,0.333333333333333,0.321975275429689,
0.333333333333333,0.321975275429689,0.333333333333333,0.321975275429689,
0.333333333333333,0.321975275429689,0.333333333333333,0.321975275429689,
0.333333333333333,0.321975275429689,0.333333333333333,0.321975275429689,
0.333333333333333,0.321975275429689,0.333333333333333,0.321975275429689,
0.333333333333333,0.321975275429689,0.333333333333333,0.321975275429689,
0.333333333333333,0.321975275429689,0.333333333333333,0.321975275429689,
0.333333333333333,0.321975275429689,0.333333333333333,0.321975275429689,
0.333333333333333,0.321975275429689,0.333333333333333,0.321975275429689,
0.333333333333333,0.321975275429689,0.333333333333333,0.321975275429689,
0.333333333333333,0.321975275429689,0.333333333333333,0.321975275429689,
0.333333333333333,0.321975275429689,0.333333333333333,0.321975275429689,
0.333333333333333,0.321975275429689,0.333333333333333,0.321975275429689,
0.333333333333333,0.321975275429689,0.333333333333333,0.321975275429689,
0.333333333333333,0.321975275429689,0.333333333333333,0.321975275429689,
0.333333333333333,0.321975275429689,0.333333333333333,0.321975275429689,
0.333333333333333,0.321975275429689,0.333333333333333,0.321975275429689,
0.333333333333333,0.321975275429689,0.333333333333333,0.321975275429689,
0.333333333333333,0.321975275429689,0.333333333333333,0.321975275429689,
0.333333333333333,0.321975275429689,0.333333333333333,0.321975275429689,
0.333333333333333,0.321975275429689,0.333333333333333,0.321975275429689,
0.333333333333333,0.321975275429689,0.333333333333333,0.321975275429689,
0.333333333333333,0.321975275429689,0.333333333333333,0.321975275429689,
0.333333333333333,0.321975275429689,0.333333333333333,0.321975275429689,
0.333333333333333,0.321975275429689,0.333333333333333,0.321975275429689,
0.333333333333333,0.321975275429689,0.333333333333333,0.321975275429689,
0.333333333333333,0.321975275429689,0.333333333333333,0.321975275429689,
0.333333333333333,0.321975275429689,0.333333333333333,0.321975275429689,
0.333333333333333,0.321975275429689,0.333333333333333,0.321975275429689,
0.333333333333333,0.321975275429689,0.333333333333333,0.321975275429689,
0.333333333333333,0.321975275429689,0.333333333333333,0.321975275429689,
0.333333333333333,0.321975275429689,0.333333333333333,0.321975275429689,
0.333333333333333,0.321975275429689,0.333333333333333,0.321975275429689,
0.333333333333333,0.321975275429689,0.333333333333333,0.321975275429689,
0.333333333333333,0.321975275429689,0.333333333333333,0.321975275429689,
0.333333333333333,0.321975275429689,0.333333333333333,0.321975275429689,
0.333333333333333,0.321975275429689,0.333333333333333,0.321975275429689,
0.333333333333333,0.321975275429689,0.333333333333333,0.321975275429689,
0.333333333333333,0.321975275429689,0.333333333333333,0.321975275429689,
0.333333333333333),(0.333333333333333,0.321975275429689,0.333333333333333,
0.321975275429689,0.333333333333333,0.321975275429689,0.333333333333333,
0.321975275429689,0.333333333333333,0.321975275429689,0.333333333333333,
0.321975275429689,0.333333333333333,0.321975275429689,0.333333333333333,
0.321975275429689,0.333333333333333,0.321975275429689,0.333333333333333,
0.321975275429689,0.333333333333333,0.321975275429689,0.333333333333333,
0.321975275429689,0.333333333333333,0.321975275429689,0.333333333333333,
0.321975275429689,0.333333333333333,0.321975275429689,0.333333333333333,
0.321975275429689,0.333333333333333,0.321975275429689,0.333333333333333,
0.321975275429689,0.333333333333333,0.321975275429689,0.333333333333333,
0.321975275429689,0.333333333333333,0.321975275429689,0.333333333333333,
0.321975275429689,0.333333333333333,0.321975275429689,0.333333333333333,
0.321975275429689,0.333333333333333,0.321975275429689,0.333333333333333,
0.321975275429689,0.333333333333333,0.321975275429689,0.333333333333333,
0.321975275429689,0.333333333333333,0.321975275429689,0.333333333333333,
0.321975275429689,0.333333333333333,0.321975275429689,0.333333333333333,
0.321975275429689,0.333333333333333,0.321975275429689,0.333333333333333,
0.321975275429689,0.333333333333333,0.321975275429689,0.333333333333333,
0.321975275429689,0.333333333333333,0.321975275429689,0.333333333333333,
0.321975275429689,0.333333333333333,0.321975275429689,0.333333333333333,
0.321975275429689,0.333333333333333,0.321975275429689,0.333333333333333,
0.321975275429689,0.333333333333333,0.321975275429689,0.333333333333333,
0.321975275429689,0.333333333333333,0.321975275429689,0.333333333333333,
0.321975275429689,0.333333333333333,0.321975275429689,0.333333333333333,
0.321975275429689,0.333333333333333,0.321975275429689,0.333333333333333,
0.321975275429689,0.333333333333333,0.321975275429689,0.333333333333333,
0.321975275429689,0.333333333333333,0.321975275429689,0.333333333333333,
0.321975275429689,0.333333333333333,0.321975275429689,0.333333333333333,
0.321975275429689,0.333333333333333,0.321975275429689,0.333333333333333,
0.321975275429689,0.333333333333333,0.321975275429689,0.333333333333333,
0.321975275429689,0.333333333333333,0.321975275429689,0.333333333333333,
0.321975275429689,0.333333333333333,0.321975275429689,0.333333333333333,
0.321975275429689,0.333333333333333,0.321975275429689,0.333333333333333,
0.321975275429689,0.333333333333333,0.321975275429689,0.333333333333333,
0.321975275429689,0.333333333333333,0.321975275429689,0.333333333333333,
0.321975275429689,0.333333333333333,0.321975275429689,0.333333333333333,
0.321975275429689,0.333333333333333,0.321975275429689,0.333333333333333,
0.321975275429689,0.333333333333333,0.321975275429689,0.333333333333333,
0.321975275429689,0.333333333333333,0.321975275429689,0.333333333333333,
0.321975275429689,0.333333333333333,0.321975275429689,0.333333333333333,
0.321975275429689,0.333333333333333,0.321975275429689,0.333333333333333,
0.321975275429689,0.333333333333333,0.321975275429689,0.333333333333333,
0.321975275429689,0.333333333333333,0.321975275429689,0.333333333333333,
0.321975275429689,0.333333333333333,0.321975275429689,0.333333333333333,
0.321975275429689,0.333333333333333,0.321975275429689,0.333333333333333,
0.321975275429689,0.333333333333333,0.321975275429689,0.333333333333333,
0.321975275429689,0.333333333333333,0.321975275429689,0.333333333333333,
0.321975275429689,0.333333333333333,0.321975275429689,0.333333333333333,
0.321975275429689,0.333333333333333),(1.,0.965925826289068,1.,0.965925826289068,
1.,0.965925826289068,1.,0.965925826289068,1.,0.965925826289068,1.,0.965925826289068,
1.,0.965925826289068,1.,0.965925826289068,1.,0.965925826289068,1.,0.965925826289068,
1.,0.965925826289068,1.,0.965925826289068,1.,0.965925826289068,1.,0.965925826289068,
1.,0.965925826289068,1.,0.965925826289068,1.,0.965925826289068,1.,0.965925826289068,
1.,0.965925826289068,1.,0.965925826289068,1.,0.965925826289068,1.,0.965925826289068,
1.,0.965925826289068,1.,0.965925826289068,1.,0.965925826289068,1.,0.965925826289068,
1.,0.965925826289068,1.,0.965925826289068,1.,0.965925826289068,1.,0.965925826289068,
1.,0.965925826289068,1.,0.965925826289068,1.,0.965925826289068,1.,0.965925826289068,
1.,0.965925826289068,1.,0.965925826289068,1.,0.965925826289068,1.,0.965925826289068,
1.,0.965925826289068,1.,0.965925826289068,1.,0.965925826289068,1.,0.965925826289068,
1.,0.965925826289068,1.,0.965925826289068,1.,0.965925826289068,1.,0.965925826289068,
1.,0.965925826289068,1.,0.965925826289068,1.,0.965925826289068,1.,0.965925826289068,
1.,0.965925826289068,1.,0.965925826289068,1.,0.965925826289068,1.,0.965925826289068,
1.,0.965925826289068,1.,0.965925826289068,1.,0.965925826289068,1.,0.965925826289068,
1.,0.965925826289068,1.,0.965925826289068,1.,0.965925826289068,1.,0.965925826289068,
1.,0.965925826289068,1.,0.965925826289068,1.,0.965925826289068,1.,0.965925826289068,
1.,0.965925826289068,1.,0.965925826289068,1.,0.965925826289068,1.,0.965925826289068,
1.,0.965925826289068,1.,0.965925826289068,1.,0.965925826289068,1.,0.965925826289068,
1.,0.965925826289068,1.,0.965925826289068,1.,0.965925826289068,1.,0.965925826289068,
1.,0.965925826289068,1.,0.965925826289068,1.,0.965925826289068,1.,0.965925826289068,
1.,0.965925826289068,1.,0.965925826289068,1.,0.965925826289068,1.,0.965925826289068,
1.,0.965925826289068,1.,0.965925826289068,1.,0.965925826289068,1.,0.965925826289068,
1.,0.965925826289068,1.,0.965925826289068,1.,0.965925826289068,1.,0.965925826289068,
1.,0.965925826289068,1.,0.965925826289068,1.)))
REPRESENTATION_ITEM('')
SURFACE()
);
#19=(
BOUNDED_SURFACE()
B_SPLINE_SURFACE(3,3,((#11307,#11308,#11309,#11310,#11311,#11312,#11313,
#11314,#11315,#11316,#11317,#11318,#11319,#11320,#11321,#11322,#11323,#11324,
#11325,#11326,#11327,#11328,#11329,#11330,#11331,#11332,#11333,#11334,#11335,
#11336,#11337,#11338,#11339,#11340,#11341,#11342,#11343,#11344,#11345,#11346),
(#11347,#11348,#11349,#11350,#11351,#11352,#11353,#11354,#11355,#11356,
#11357,#11358,#11359,#11360,#11361,#11362,#11363,#11364,#11365,#11366,#11367,
#11368,#11369,#11370,#11371,#11372,#11373,#11374,#11375,#11376,#11377,#11378,
#11379,#11380,#11381,#11382,#11383,#11384,#11385,#11386),(#11387,#11388,
#11389,#11390,#11391,#11392,#11393,#11394,#11395,#11396,#11397,#11398,#11399,
#11400,#11401,#11402,#11403,#11404,#11405,#11406,#11407,#11408,#11409,#11410,
#11411,#11412,#11413,#11414,#11415,#11416,#11417,#11418,#11419,#11420,#11421,
#11422,#11423,#11424,#11425,#11426),(#11427,#11428,#11429,#11430,#11431,
#11432,#11433,#11434,#11435,#11436,#11437,#11438,#11439,#11440,#11441,#11442,
#11443,#11444,#11445,#11446,#11447,#11448,#11449,#11450,#11451,#11452,#11453,
#11454,#11455,#11456,#11457,#11458,#11459,#11460,#11461,#11462,#11463,#11464,
#11465,#11466),(#11467,#11468,#11469,#11470,#11471,#11472,#11473,#11474,
#11475,#11476,#11477,#11478,#11479,#11480,#11481,#11482,#11483,#11484,#11485,
#11486,#11487,#11488,#11489,#11490,#11491,#11492,#11493,#11494,#11495,#11496,
#11497,#11498,#11499,#11500,#11501,#11502,#11503,#11504,#11505,#11506),
(#11507,#11508,#11509,#11510,#11511,#11512,#11513,#11514,#11515,#11516,
#11517,#11518,#11519,#11520,#11521,#11522,#11523,#11524,#11525,#11526,#11527,
#11528,#11529,#11530,#11531,#11532,#11533,#11534,#11535,#11536,#11537,#11538,
#11539,#11540,#11541,#11542,#11543,#11544,#11545,#11546),(#11547,#11548,
#11549,#11550,#11551,#11552,#11553,#11554,#11555,#11556,#11557,#11558,#11559,
#11560,#11561,#11562,#11563,#11564,#11565,#11566,#11567,#11568,#11569,#11570,
#11571,#11572,#11573,#11574,#11575,#11576,#11577,#11578,#11579,#11580,#11581,
#11582,#11583,#11584,#11585,#11586)),.UNSPECIFIED.,.T.,.F.,.F.)
B_SPLINE_SURFACE_WITH_KNOTS((4,3,4),(4,2,2,2,2,2,2,2,2,2,2,2,2,2,2,2,2,
2,2,4),(0.,0.5,1.),(-2.95233260527408E-7,0.0437517296050676,0.0875034592101352,
0.131255188815203,0.17500691842027,0.196882783222804,0.218758648025338,
0.262510377630406,0.350013836840541,0.418185084306465,0.486356331772389,
0.554527579238313,0.622698826704237,0.669861473366207,0.717024120028178,
0.811349413352118,0.858512060014089,0.905674706676059,0.95283735333803,
1.),.UNSPECIFIED.)
GEOMETRIC_REPRESENTATION_ITEM()
RATIONAL_B_SPLINE_SURFACE(((1.,1.,1.,1.,1.,1.,1.,1.,1.,1.,1.,1.,1.,1.,1.,
1.,1.,1.,1.,1.,1.,1.,1.,1.,1.,1.,1.,1.,1.,1.,1.,1.,1.,1.,1.,1.,1.,1.,1.,
1.),(0.333333333333334,0.333333333333333,0.333333333333333,0.333333333333333,
0.333333333333333,0.333333333333333,0.333333333333333,0.333333333333333,
0.333333333333333,0.333333333333333,0.333333333333333,0.333333333333333,
0.333333333333333,0.333333333333333,0.333333333333333,0.333333333333333,
0.333333333333333,0.333333333333333,0.333333333333333,0.333333333333333,
0.333333333333333,0.333333333333333,0.333333333333333,0.333333333333333,
0.333333333333333,0.333333333333333,0.333333333333333,0.333333333333333,
0.333333333333333,0.333333333333333,0.333333333333333,0.333333333333333,
0.333333333333333,0.333333333333333,0.333333333333333,0.333333333333333,
0.333333333333333,0.333333333333333,0.333333333333333,0.333333333333333),
(0.333333333333334,0.333333333333333,0.333333333333333,0.333333333333333,
0.333333333333333,0.333333333333333,0.333333333333333,0.333333333333333,
0.333333333333333,0.333333333333333,0.333333333333333,0.333333333333333,
0.333333333333333,0.333333333333333,0.333333333333333,0.333333333333333,
0.333333333333333,0.333333333333333,0.333333333333333,0.333333333333333,
0.333333333333333,0.333333333333333,0.333333333333333,0.333333333333333,
0.333333333333333,0.333333333333333,0.333333333333333,0.333333333333333,
0.333333333333333,0.333333333333333,0.333333333333333,0.333333333333333,
0.333333333333333,0.333333333333333,0.333333333333333,0.333333333333333,
0.333333333333333,0.333333333333333,0.333333333333333,0.333333333333333),
(1.,1.,1.,1.,1.,1.,1.,1.,1.,1.,1.,1.,1.,1.,1.,1.,1.,1.,1.,1.,1.,1.,1.,1.,
1.,1.,1.,1.,1.,1.,1.,1.,1.,1.,1.,1.,1.,1.,1.,1.),(0.333333333333334,0.333333333333333,
0.333333333333333,0.333333333333333,0.333333333333333,0.333333333333333,
0.333333333333333,0.333333333333333,0.333333333333333,0.333333333333333,
0.333333333333333,0.333333333333333,0.333333333333333,0.333333333333333,
0.333333333333333,0.333333333333333,0.333333333333333,0.333333333333333,
0.333333333333333,0.333333333333333,0.333333333333333,0.333333333333333,
0.333333333333333,0.333333333333333,0.333333333333333,0.333333333333333,
0.333333333333333,0.333333333333333,0.333333333333333,0.333333333333333,
0.333333333333333,0.333333333333333,0.333333333333333,0.333333333333333,
0.333333333333333,0.333333333333333,0.333333333333333,0.333333333333333,
0.333333333333333,0.333333333333333),(0.333333333333334,0.333333333333333,
0.333333333333333,0.333333333333333,0.333333333333333,0.333333333333333,
0.333333333333333,0.333333333333333,0.333333333333333,0.333333333333333,
0.333333333333333,0.333333333333333,0.333333333333333,0.333333333333333,
0.333333333333333,0.333333333333333,0.333333333333333,0.333333333333333,
0.333333333333333,0.333333333333333,0.333333333333333,0.333333333333333,
0.333333333333333,0.333333333333333,0.333333333333333,0.333333333333333,
0.333333333333333,0.333333333333333,0.333333333333333,0.333333333333333,
0.333333333333333,0.333333333333333,0.333333333333333,0.333333333333333,
0.333333333333333,0.333333333333333,0.333333333333333,0.333333333333333,
0.333333333333333,0.333333333333333),(1.,1.,1.,1.,1.,1.,1.,1.,1.,1.,1.,
1.,1.,1.,1.,1.,1.,1.,1.,1.,1.,1.,1.,1.,1.,1.,1.,1.,1.,1.,1.,1.,1.,1.,1.,
1.,1.,1.,1.,1.)))
REPRESENTATION_ITEM('')
SURFACE()
);
#20=(
BOUNDED_SURFACE()
B_SPLINE_SURFACE(3,3,((#11593,#11594,#11595,#11596,#11597,#11598,#11599,
#11600,#11601,#11602,#11603,#11604),(#11605,#11606,#11607,#11608,#11609,
#11610,#11611,#11612,#11613,#11614,#11615,#11616),(#11617,#11618,#11619,
#11620,#11621,#11622,#11623,#11624,#11625,#11626,#11627,#11628),(#11629,
#11630,#11631,#11632,#11633,#11634,#11635,#11636,#11637,#11638,#11639,#11640),
(#11641,#11642,#11643,#11644,#11645,#11646,#11647,#11648,#11649,#11650,
#11651,#11652),(#11653,#11654,#11655,#11656,#11657,#11658,#11659,#11660,
#11661,#11662,#11663,#11664),(#11665,#11666,#11667,#11668,#11669,#11670,
#11671,#11672,#11673,#11674,#11675,#11676)),.UNSPECIFIED.,.T.,.F.,.F.)
B_SPLINE_SURFACE_WITH_KNOTS((4,3,4),(4,2,2,2,2,4),(0.,0.5,1.),(0.727251200985696,
0.761344800862484,0.795438400739272,0.863625600492848,0.931812800246424,
1.),.UNSPECIFIED.)
GEOMETRIC_REPRESENTATION_ITEM()
RATIONAL_B_SPLINE_SURFACE(((1.,1.,1.,1.,1.,1.,1.,1.,1.,1.,1.,1.),(0.333333333333333,
0.333333333333333,0.333333333333333,0.333333333333333,0.333333333333333,
0.333333333333333,0.333333333333333,0.333333333333333,0.333333333333333,
0.333333333333333,0.333333333333333,0.333333333333333),(0.333333333333333,
0.333333333333333,0.333333333333333,0.333333333333333,0.333333333333333,
0.333333333333333,0.333333333333333,0.333333333333333,0.333333333333333,
0.333333333333333,0.333333333333333,0.333333333333333),(1.,1.,1.,1.,1.,
1.,1.,1.,1.,1.,1.,1.),(0.333333333333333,0.333333333333333,0.333333333333333,
0.333333333333333,0.333333333333333,0.333333333333333,0.333333333333333,
0.333333333333333,0.333333333333333,0.333333333333333,0.333333333333333,
0.333333333333333),(0.333333333333333,0.333333333333333,0.333333333333333,
0.333333333333333,0.333333333333333,0.333333333333333,0.333333333333333,
0.333333333333333,0.333333333333333,0.333333333333333,0.333333333333333,
0.333333333333333),(1.,1.,1.,1.,1.,1.,1.,1.,1.,1.,1.,1.)))
REPRESENTATION_ITEM('')
SURFACE()
);
#21=ITEM_DEFINED_TRANSFORMATION($,$,#2014,#2046);
#22=ITEM_DEFINED_TRANSFORMATION($,$,#2022,#2047);
#23=ITEM_DEFINED_TRANSFORMATION($,$,#2036,#2048);
#24=ITEM_DEFINED_TRANSFORMATION($,$,#1962,#2148);
#25=ITEM_DEFINED_TRANSFORMATION($,$,#1997,#2149);
#26=ITEM_DEFINED_TRANSFORMATION($,$,#2115,#2150);
#27=ITEM_DEFINED_TRANSFORMATION($,$,#2131,#2151);
#28=ITEM_DEFINED_TRANSFORMATION($,$,#2005,#2152);
#29=ITEM_DEFINED_TRANSFORMATION($,$,#2013,#2153);
#30=ITEM_DEFINED_TRANSFORMATION($,$,#2049,#2154);
#31=ITEM_DEFINED_TRANSFORMATION($,$,#2074,#2155);
#32=ITEM_DEFINED_TRANSFORMATION($,$,#2080,#2156);
#33=ITEM_DEFINED_TRANSFORMATION($,$,#2131,#2157);
#34=ITEM_DEFINED_TRANSFORMATION($,$,#2115,#2158);
#35=ITEM_DEFINED_TRANSFORMATION($,$,#2131,#2159);
#36=(
REPRESENTATION_RELATIONSHIP($,$,#12188,#12187)
REPRESENTATION_RELATIONSHIP_WITH_TRANSFORMATION(#21)
SHAPE_REPRESENTATION_RELATIONSHIP()
);
#37=(
REPRESENTATION_RELATIONSHIP($,$,#12189,#12187)
REPRESENTATION_RELATIONSHIP_WITH_TRANSFORMATION(#22)
SHAPE_REPRESENTATION_RELATIONSHIP()
);
#38=(
REPRESENTATION_RELATIONSHIP($,$,#12190,#12187)
REPRESENTATION_RELATIONSHIP_WITH_TRANSFORMATION(#23)
SHAPE_REPRESENTATION_RELATIONSHIP()
);
#39=(
REPRESENTATION_RELATIONSHIP($,$,#12184,#12183)
REPRESENTATION_RELATIONSHIP_WITH_TRANSFORMATION(#24)
SHAPE_REPRESENTATION_RELATIONSHIP()
);
#40=(
REPRESENTATION_RELATIONSHIP($,$,#12185,#12183)
REPRESENTATION_RELATIONSHIP_WITH_TRANSFORMATION(#25)
SHAPE_REPRESENTATION_RELATIONSHIP()
);
#41=(
REPRESENTATION_RELATIONSHIP($,$,#12194,#12183)
REPRESENTATION_RELATIONSHIP_WITH_TRANSFORMATION(#26)
SHAPE_REPRESENTATION_RELATIONSHIP()
);
#42=(
REPRESENTATION_RELATIONSHIP($,$,#12195,#12183)
REPRESENTATION_RELATIONSHIP_WITH_TRANSFORMATION(#27)
SHAPE_REPRESENTATION_RELATIONSHIP()
);
#43=(
REPRESENTATION_RELATIONSHIP($,$,#12186,#12183)
REPRESENTATION_RELATIONSHIP_WITH_TRANSFORMATION(#28)
SHAPE_REPRESENTATION_RELATIONSHIP()
);
#44=(
REPRESENTATION_RELATIONSHIP($,$,#12187,#12183)
REPRESENTATION_RELATIONSHIP_WITH_TRANSFORMATION(#29)
SHAPE_REPRESENTATION_RELATIONSHIP()
);
#45=(
REPRESENTATION_RELATIONSHIP($,$,#12191,#12183)
REPRESENTATION_RELATIONSHIP_WITH_TRANSFORMATION(#30)
SHAPE_REPRESENTATION_RELATIONSHIP()
);
#46=(
REPRESENTATION_RELATIONSHIP($,$,#12192,#12183)
REPRESENTATION_RELATIONSHIP_WITH_TRANSFORMATION(#31)
SHAPE_REPRESENTATION_RELATIONSHIP()
);
#47=(
REPRESENTATION_RELATIONSHIP($,$,#12193,#12183)
REPRESENTATION_RELATIONSHIP_WITH_TRANSFORMATION(#32)
SHAPE_REPRESENTATION_RELATIONSHIP()
);
#48=(
REPRESENTATION_RELATIONSHIP($,$,#12195,#12183)
REPRESENTATION_RELATIONSHIP_WITH_TRANSFORMATION(#33)
SHAPE_REPRESENTATION_RELATIONSHIP()
);
#49=(
REPRESENTATION_RELATIONSHIP($,$,#12194,#12183)
REPRESENTATION_RELATIONSHIP_WITH_TRANSFORMATION(#34)
SHAPE_REPRESENTATION_RELATIONSHIP()
);
#50=(
REPRESENTATION_RELATIONSHIP($,$,#12195,#12183)
REPRESENTATION_RELATIONSHIP_WITH_TRANSFORMATION(#35)
SHAPE_REPRESENTATION_RELATIONSHIP()
);
#51=CONTEXT_DEPENDENT_SHAPE_REPRESENTATION(#36,#12163);
#52=CONTEXT_DEPENDENT_SHAPE_REPRESENTATION(#37,#12164);
#53=CONTEXT_DEPENDENT_SHAPE_REPRESENTATION(#38,#12165);
#54=CONTEXT_DEPENDENT_SHAPE_REPRESENTATION(#39,#12171);
#55=CONTEXT_DEPENDENT_SHAPE_REPRESENTATION(#40,#12172);
#56=CONTEXT_DEPENDENT_SHAPE_REPRESENTATION(#41,#12173);
#57=CONTEXT_DEPENDENT_SHAPE_REPRESENTATION(#42,#12174);
#58=CONTEXT_DEPENDENT_SHAPE_REPRESENTATION(#43,#12175);
#59=CONTEXT_DEPENDENT_SHAPE_REPRESENTATION(#44,#12176);
#60=CONTEXT_DEPENDENT_SHAPE_REPRESENTATION(#45,#12177);
#61=CONTEXT_DEPENDENT_SHAPE_REPRESENTATION(#46,#12178);
#62=CONTEXT_DEPENDENT_SHAPE_REPRESENTATION(#47,#12179);
#63=CONTEXT_DEPENDENT_SHAPE_REPRESENTATION(#48,#12180);
#64=CONTEXT_DEPENDENT_SHAPE_REPRESENTATION(#49,#12181);
#65=CONTEXT_DEPENDENT_SHAPE_REPRESENTATION(#50,#12182);
#66=NEXT_ASSEMBLY_USAGE_OCCURRENCE('Blade_1:1','Blade_1:1','Blade_1:1',
#12201,#12202,'Blade_1:1');
#67=NEXT_ASSEMBLY_USAGE_OCCURRENCE('Blade_2:1','Blade_2:1','Blade_2:1',
#12201,#12203,'Blade_2:1');
#68=NEXT_ASSEMBLY_USAGE_OCCURRENCE('small pin:1','small pin:1',
'small pin:1',#12201,#12204,'small pin:1');
#69=NEXT_ASSEMBLY_USAGE_OCCURRENCE('Front Cover:1','Front Cover:1',
'Front Cover:1',#12197,#12198,'Front Cover:1');
#70=NEXT_ASSEMBLY_USAGE_OCCURRENCE('knife:1','knife:1','knife:1',#12197,
#12199,'knife:1');
#71=NEXT_ASSEMBLY_USAGE_OCCURRENCE('Big pin:1','Big pin:1','Big pin:1',
#12197,#12208,'Big pin:1');
#72=NEXT_ASSEMBLY_USAGE_OCCURRENCE('Pivot spacer:1','Pivot spacer:1',
'Pivot spacer:1',#12197,#12209,'Pivot spacer:1');
#73=NEXT_ASSEMBLY_USAGE_OCCURRENCE('Knife small:1','Knife small:1',
'Knife small:1',#12197,#12200,'Knife small:1');
#74=NEXT_ASSEMBLY_USAGE_OCCURRENCE('Scissors:1','Scissors:1',
'Scissors:1',#12197,#12201,'Scissors:1');
#75=NEXT_ASSEMBLY_USAGE_OCCURRENCE('Corkscrew:1','Corkscrew:1',
'Corkscrew:1',#12197,#12205,'Corkscrew:1');
#76=NEXT_ASSEMBLY_USAGE_OCCURRENCE('Bottle opener:1','Bottle opener:1',
'Bottle opener:1',#12197,#12206,'Bottle opener:1');
#77=NEXT_ASSEMBLY_USAGE_OCCURRENCE('Back cover:1','Back cover:1',
'Back cover:1',#12197,#12207,'Back cover:1');
#78=NEXT_ASSEMBLY_USAGE_OCCURRENCE('Pivot spacer:2','Pivot spacer:2',
'Pivot spacer:2',#12197,#12209,'Pivot spacer:2');
#79=NEXT_ASSEMBLY_USAGE_OCCURRENCE('Big pin:2','Big pin:2','Big pin:2',
#12197,#12208,'Big pin:2');
#80=NEXT_ASSEMBLY_USAGE_OCCURRENCE('Pivot spacer:3','Pivot spacer:3',
'Pivot spacer:3',#12197,#12209,'Pivot spacer:3');
#81=B_SPLINE_CURVE_WITH_KNOTS('',3,(#2753,#2754,#2755,#2756,#2757,#2758,
#2759,#2760,#2761,#2762,#2763,#2764),.UNSPECIFIED.,.F.,.F.,(4,1,1,1,1,1,
1,1,1,4),(0.692277335272932,0.69714998216664,0.713058394872634,0.723664003343296,
0.736358399716042,0.759577826910316,0.780092040409136,0.810242072545427,
0.901462701662728,0.958125874426747),.UNSPECIFIED.);
#82=B_SPLINE_CURVE_WITH_KNOTS('',3,(#2768,#2769,#2770,#2771,#2772,#2773,
#2774,#2775,#2776,#2777,#2778,#2779),.UNSPECIFIED.,.F.,.F.,(4,1,1,1,1,1,
1,1,1,4),(0.692277335272932,0.69714998216664,0.713058394872634,0.723664003343296,
0.736358399716042,0.759577826910316,0.780092040409136,0.810242072545427,
0.901462701662728,0.958125874426747),.UNSPECIFIED.);
#83=B_SPLINE_CURVE_WITH_KNOTS('',3,(#2794,#2795,#2796,#2797,#2798,#2799),
 .UNSPECIFIED.,.F.,.F.,(4,1,1,4),(0.,0.587279823509184,0.66516934088919,
1.),.UNSPECIFIED.);
#84=B_SPLINE_CURVE_WITH_KNOTS('',3,(#2802,#2803,#2804,#2805,#2806,#2807),
 .UNSPECIFIED.,.F.,.F.,(4,1,1,4),(0.,0.587279823509184,0.66516934088919,
1.),.UNSPECIFIED.);
#85=B_SPLINE_CURVE_WITH_KNOTS('',3,(#2823,#2824,#2825,#2826,#2827,#2828,
#2829),.UNSPECIFIED.,.F.,.F.,(4,1,1,1,4),(0.,0.0866729836098282,0.459841695939614,
0.649673299675604,0.845208562818702),.UNSPECIFIED.);
#86=B_SPLINE_CURVE_WITH_KNOTS('',3,(#2831,#2832,#2833,#2834,#2835,#2836,
#2837),.UNSPECIFIED.,.F.,.F.,(4,3,4),(1.35324872955864E-8,0.631650088317911,
1.),.UNSPECIFIED.);
#87=B_SPLINE_CURVE_WITH_KNOTS('',3,(#2838,#2839,#2840,#2841,#2842,#2843,
#2844),.UNSPECIFIED.,.F.,.F.,(4,1,1,1,4),(0.,0.0866729836098282,0.459841695939614,
0.649673299675604,0.829767002127536),.UNSPECIFIED.);
#88=B_SPLINE_CURVE_WITH_KNOTS('',3,(#2847,#2848,#2849,#2850,#2851,#2852,
#2853,#2854,#2855,#2856,#2857,#2858,#2859,#2860,#2861,#2862,#2863,#2864,
#2865,#2866,#2867,#2868,#2869,#2870,#2871,#2872,#2873,#2874,#2875,#2876,
#2877,#2878,#2879,#2880,#2881,#2882,#2883,#2884,#2885,#2886,#2887,#2888,
#2889,#2890,#2891,#2892,#2893,#2894,#2895,#2896,#2897,#2898,#2899,#2900,
#2901,#2902,#2903,#2904,#2905,#2906,#2907,#2908,#2909,#2910,#2911,#2912,
#2913,#2914,#2915,#2916,#2917,#2918,#2919,#2920,#2921,#2922,#2923,#2924,
#2925,#2926,#2927,#2928,#2929,#2930,#2931,#2932,#2933,#2934,#2935,#2936,
#2937,#2938,#2939,#2940,#2941,#2942,#2943,#2944,#2945,#2946,#2947,#2948,
#2949,#2950,#2951,#2952,#2953,#2954,#2955,#2956,#2957,#2958,#2959,#2960,
#2961,#2962,#2963,#2964,#2965,#2966,#2967,#2968,#2969,#2970,#2971,#2972,
#2973,#2974,#2975,#2976,#2977,#2978,#2979,#2980,#2981,#2982,#2983,#2984,
#2985,#2986,#2987,#2988,#2989,#2990,#2991,#2992,#2993,#2994,#2995,#2996,
#2997,#2998,#2999,#3000,#3001,#3002,#3003,#3004,#3005,#3006,#3007,#3008,
#3009,#3010,#3011,#3012,#3013,#3014,#3015,#3016,#3017,#3018,#3019,#3020,
#3021,#3022,#3023,#3024,#3025,#3026,#3027,#3028,#3029,#3030,#3031,#3032,
#3033,#3034,#3035,#3036,#3037,#3038,#3039,#3040,#3041,#3042,#3043,#3044,
#3045,#3046,#3047,#3048,#3049,#3050,#3051,#3052,#3053,#3054,#3055,#3056,
#3057,#3058,#3059,#3060,#3061,#3062,#3063,#3064,#3065,#3066,#3067,#3068,
#3069,#3070,#3071,#3072,#3073,#3074,#3075,#3076,#3077,#3078,#3079,#3080,
#3081,#3082,#3083,#3084,#3085,#3086,#3087,#3088,#3089,#3090,#3091,#3092,
#3093,#3094,#3095,#3096,#3097,#3098,#3099,#3100,#3101,#3102,#3103,#3104,
#3105,#3106,#3107,#3108,#3109,#3110,#3111,#3112,#3113,#3114,#3115,#3116,
#3117,#3118,#3119,#3120,#3121,#3122,#3123,#3124,#3125,#3126,#3127,#3128,
#3129,#3130,#3131,#3132,#3133,#3134,#3135,#3136,#3137,#3138,#3139,#3140,
#3141,#3142,#3143,#3144,#3145,#3146,#3147,#3148,#3149,#3150,#3151,#3152,
#3153,#3154,#3155,#3156,#3157,#3158,#3159,#3160,#3161,#3162,#3163,#3164,
#3165,#3166,#3167,#3168,#3169,#3170,#3171,#3172,#3173,#3174,#3175,#3176,
#3177),.UNSPECIFIED.,.F.,.F.,(4,3,3,3,3,3,3,3,3,3,3,3,3,3,3,3,3,3,3,3,3,
3,3,3,3,3,3,3,3,3,3,3,3,3,3,3,3,3,3,3,3,3,3,3,3,3,3,3,3,3,3,3,3,3,3,3,3,
3,3,3,3,3,3,3,3,3,3,3,3,3,3,3,3,3,3,3,3,3,3,3,3,3,3,3,3,3,3,3,3,3,3,3,3,
3,3,3,3,3,3,3,3,3,3,3,3,3,3,3,3,3,4),(1.00000005226737E-6,0.00728562366971475,
0.0234463959847306,0.0557978953419903,0.0881792075542466,0.120578085908497,
0.199435146924132,0.250102975200852,0.332264327598246,0.378931394146745,
0.442710847956035,0.458655711408358,0.465225430544162,0.470485225689555,
0.506490301765326,0.587406978409983,0.63447750239409,0.698713581314966,
0.762996361968068,0.827238553299382,0.891353412993002,0.919885897936909,
0.925235738863892,0.927910373024815,0.929197830974231,0.93032386627772,
0.965310836068324,1.00172317218786,1.00548335276863,1.0439300169432,1.08610137935927,
1.14148474424288,1.17398141008201,1.20363917088317,1.23143564581068,1.25060619127644,
1.27597878060136,1.29260925110888,1.33079359731686,1.3485547264891,1.3496219232794,
1.35038687476659,1.36631585566134,1.43886146909154,1.48931728875302,1.51524396218266,
1.57648663203031,1.5962584262802,1.66704233666681,1.6830136697589,1.74924243686783,
1.77713875907306,1.81979916869953,1.82771178722931,1.87226124160844,1.8812062035948,
1.92683921666331,1.96328819238212,1.98151268024153,1.99062492417124,1.99518104613609,
1.99809663447909,1.99973716810094,2.11425198948044,2.25593468219522,2.3831520244116,
2.49139452866391,2.51036936662798,2.54228741890446,2.56622595811182,2.57160131643996,
2.57333509499776,2.63448414790964,2.63804157573391,2.70877992194418,2.77951826815446,
2.85750983652355,2.92223429974548,2.94135846274582,3.00435550993043,3.07158275602607,
3.13078242154972,3.20465260936858,3.28573698285387,3.35844860482519,3.42587818692828,
3.4764503735056,3.48117348962947,3.48410509148297,3.62816693323756,3.7643950388047,
3.88405944557012,3.90062314437185,4.00766553231559,4.10852611031876,4.17975199447887,
4.27429663966353,4.32614318790147,4.41732790628579,4.48050879966944,4.56192648809965,
4.60400180805684,4.64714550046042,4.69150379518099,4.73725365207584,4.7884515645196,
4.83385532714358,4.88768324231123,4.93951305213049,4.99975507375154,5.03337263030683),
 .UNSPECIFIED.);
#89=B_SPLINE_CURVE_WITH_KNOTS('',3,(#3186,#3187,#3188,#3189,#3190,#3191,
#3192,#3193,#3194,#3195,#3196,#3197,#3198,#3199,#3200,#3201,#3202,#3203,
#3204,#3205,#3206,#3207,#3208,#3209,#3210,#3211,#3212,#3213,#3214,#3215,
#3216,#3217,#3218,#3219,#3220,#3221,#3222,#3223,#3224,#3225,#3226,#3227,
#3228,#3229,#3230,#3231,#3232,#3233,#3234,#3235,#3236,#3237,#3238,#3239,
#3240,#3241,#3242,#3243,#3244,#3245,#3246,#3247,#3248,#3249,#3250,#3251,
#3252,#3253,#3254,#3255,#3256,#3257,#3258,#3259,#3260,#3261,#3262,#3263,
#3264,#3265,#3266,#3267,#3268,#3269,#3270,#3271,#3272,#3273,#3274,#3275,
#3276,#3277,#3278,#3279,#3280,#3281,#3282,#3283,#3284,#3285,#3286,#3287,
#3288,#3289,#3290,#3291,#3292,#3293,#3294,#3295,#3296),.UNSPECIFIED.,.F.,
 .F.,(4,2,2,2,2,1,2,2,2,2,2,2,2,2,2,2,2,2,2,2,2,2,2,2,2,2,2,2,2,2,2,2,2,
2,2,2,2,2,2,2,2,2,2,2,2,2,2,2,2,2,2,2,2,2,2,4),(0.,0.000220711532429116,
0.000489265959006191,0.00102637481216034,0.00156348366531445,0.0026377013716227,
0.003711919077931,0.00586035449054751,0.0101572253157805,0.0144540961410136,
0.0187509669662467,0.0359384502671788,0.0531259335681111,0.0703134168690433,
0.0875009001699755,0.0960946418204416,0.104688383470908,0.113282125121374,
0.12187586677184,0.139063350072772,0.156250833373704,0.190625799975569,
0.207813283276501,0.225000766577433,0.242188249878365,0.259375733179298,
0.293750699781162,0.328125666383026,0.362500632984891,0.396875599586755,
0.43125056618862,0.448438049489552,0.465625532790484,0.500000499392348,
0.568750432596077,0.637500365799806,0.67187533240167,0.706250299003535,
0.723437782304467,0.740625265605399,0.775000232207264,0.809375198809128,
0.843750165410992,0.878125132012857,0.912500098614721,0.929687581915653,
0.946875065216586,0.955468806867052,0.959765677692285,0.964062548517518,
0.968359419342751,0.972656290167984,0.98125003181845,0.989843773468916,
0.998437515119382,0.999999994546672),.UNSPECIFIED.);
#90=B_SPLINE_CURVE_WITH_KNOTS('',3,(#3298,#3299,#3300,#3301,#3302,#3303),
 .UNSPECIFIED.,.F.,.F.,(4,2,4),(9.43755849736976E-11,0.103884415747993,
0.213656518400476),.UNSPECIFIED.);
#91=B_SPLINE_CURVE_WITH_KNOTS('',3,(#3645,#3646,#3647,#3648,#3649,#3650,
#3651,#3652),.UNSPECIFIED.,.F.,.F.,(4,1,1,1,1,4),(0.,0.0142399187551309,
0.253552302413509,0.548288200579205,0.757181970713106,0.999999999751732),
 .UNSPECIFIED.);
#92=B_SPLINE_CURVE_WITH_KNOTS('',3,(#3655,#3656,#3657,#3658,#3659,#3660,
#3661,#3662),.UNSPECIFIED.,.F.,.F.,(4,1,1,1,1,4),(0.,0.156258367612318,
0.290685780689375,0.48035435867502,0.63435677163295,0.643520450566124),
 .UNSPECIFIED.);
#93=B_SPLINE_CURVE_WITH_KNOTS('',3,(#3689,#3690,#3691,#3692,#3693,#3694,
#3695,#3696),.UNSPECIFIED.,.F.,.F.,(4,1,1,1,1,4),(0.736469307506587,0.759577826910316,
0.780092040409136,0.810242072545427,0.901462701662728,0.958125874426747),
 .UNSPECIFIED.);
#94=B_SPLINE_CURVE_WITH_KNOTS('',3,(#3698,#3699,#3700,#3701,#3702,#3703,
#3704,#3705,#3706,#3707,#3708,#3709,#3710,#3711,#3712,#3713,#3714,#3715,
#3716,#3717,#3718,#3719,#3720,#3721,#3722,#3723,#3724,#3725,#3726,#3727,
#3728,#3729,#3730,#3731,#3732,#3733,#3734,#3735,#3736,#3737,#3738,#3739,
#3740,#3741,#3742,#3743,#3744,#3745,#3746,#3747,#3748,#3749,#3750,#3751,
#3752,#3753,#3754,#3755,#3756,#3757,#3758,#3759,#3760,#3761,#3762,#3763,
#3764,#3765,#3766,#3767,#3768,#3769,#3770,#3771,#3772,#3773,#3774,#3775,
#3776,#3777,#3778,#3779,#3780,#3781,#3782,#3783,#3784,#3785,#3786,#3787,
#3788,#3789,#3790,#3791,#3792,#3793,#3794,#3795,#3796,#3797,#3798,#3799,
#3800,#3801,#3802,#3803,#3804,#3805,#3806,#3807,#3808,#3809,#3810,#3811,
#3812,#3813,#3814,#3815,#3816,#3817,#3818,#3819,#3820,#3821,#3822,#3823,
#3824,#3825,#3826,#3827,#3828,#3829,#3830),.UNSPECIFIED.,.F.,.F.,(4,3,3,
3,3,3,3,3,3,3,3,3,3,3,3,3,3,3,3,3,3,3,3,3,3,3,3,3,3,3,3,3,3,3,3,3,3,3,3,
3,3,3,3,3,4),(-0.304790736556663,-0.304217640980641,-0.296038101920973,
-0.286515952540819,-0.273360133864138,-0.263801143460453,-0.260204315187458,
-0.252535972236165,-0.245519918591342,-0.239298827086652,-0.23653215327504,
-0.233416187936625,-0.215837477852405,-0.203856027214574,-0.191047566863345,
-0.175753773870387,-0.174731606854691,-0.162449438164595,-0.154804922668266,
-0.148252398403841,-0.141338529588791,-0.14102776216038,-0.126737062057896,
-0.12479373531637,-0.116512797864951,-0.111129032227751,-0.108231860413532,
-0.0915022809864805,-0.0886339189716657,-0.0739698737112559,-0.0661726083847358,
-0.0615130055232586,-0.0515620766849569,-0.0423955634704539,-0.0412018838190183,
-0.035176421754689,-0.0328794524142148,-0.0289001906178499,-0.025349772457395,
-0.0253217992573334,-0.0232012051308284,-0.017145962928431,-0.0130970487849195,
-0.00238990525332499,-9.99999152508124E-7),.UNSPECIFIED.);
#95=B_SPLINE_CURVE_WITH_KNOTS('',3,(#3834,#3835,#3836,#3837,#3838,#3839,
#3840,#3841,#3842,#3843,#3844,#3845),.UNSPECIFIED.,.F.,.F.,(4,1,1,1,1,1,
1,1,1,4),(0.69268150065498,0.69714998216664,0.713058394872634,0.723664003343296,
0.736358399716042,0.759577826910316,0.780092040409136,0.810242072545427,
0.901462701662728,0.958125874426747),.UNSPECIFIED.);
#96=B_SPLINE_CURVE_WITH_KNOTS('',3,(#3860,#3861,#3862,#3863,#3864,#3865),
 .UNSPECIFIED.,.F.,.F.,(4,1,1,4),(0.,0.587279823509184,0.66516934088919,
1.),.UNSPECIFIED.);
#97=B_SPLINE_CURVE_WITH_KNOTS('',3,(#3868,#3869,#3870,#3871,#3872,#3873),
 .UNSPECIFIED.,.F.,.F.,(4,1,1,4),(0.,0.587279823509184,0.66516934088919,
1.),.UNSPECIFIED.);
#98=B_SPLINE_CURVE_WITH_KNOTS('',3,(#3889,#3890,#3891,#3892,#3893,#3894,
#3895),.UNSPECIFIED.,.F.,.F.,(4,3,4),(-0.142199063954041,-0.0695096318207944,
0.),.UNSPECIFIED.);
#99=B_SPLINE_CURVE_WITH_KNOTS('',3,(#3896,#3897,#3898,#3899,#3900,#3901,
#3902),.UNSPECIFIED.,.F.,.F.,(4,1,1,1,4),(0.,0.0866729836098282,0.459841695939614,
0.649673299675604,0.828039681548554),.UNSPECIFIED.);
#100=B_SPLINE_CURVE_WITH_KNOTS('',3,(#3903,#3904,#3905,#3906,#3907,#3908,
#3909),.UNSPECIFIED.,.F.,.F.,(4,1,1,1,4),(0.,0.0866729836098282,0.459841695939614,
0.649673299675604,0.845208563176808),.UNSPECIFIED.);
#101=B_SPLINE_CURVE_WITH_KNOTS('',3,(#3911,#3912,#3913,#3914,#3915,#3916,
#3917,#3918,#3919,#3920,#3921,#3922,#3923,#3924,#3925,#3926,#3927,#3928,
#3929,#3930,#3931,#3932,#3933,#3934,#3935,#3936,#3937,#3938,#3939,#3940,
#3941,#3942,#3943,#3944,#3945,#3946,#3947,#3948,#3949,#3950,#3951,#3952,
#3953,#3954,#3955,#3956,#3957,#3958,#3959,#3960,#3961,#3962,#3963,#3964,
#3965,#3966,#3967,#3968,#3969,#3970,#3971,#3972,#3973,#3974,#3975,#3976,
#3977,#3978,#3979,#3980,#3981,#3982,#3983,#3984,#3985,#3986,#3987,#3988,
#3989,#3990,#3991,#3992,#3993,#3994,#3995,#3996,#3997,#3998,#3999,#4000,
#4001,#4002,#4003,#4004,#4005,#4006,#4007,#4008,#4009,#4010,#4011,#4012,
#4013,#4014,#4015,#4016,#4017,#4018,#4019,#4020,#4021,#4022,#4023,#4024,
#4025,#4026,#4027,#4028,#4029,#4030,#4031,#4032,#4033,#4034,#4035,#4036,
#4037,#4038,#4039,#4040,#4041,#4042,#4043,#4044,#4045,#4046,#4047,#4048,
#4049,#4050,#4051,#4052,#4053,#4054,#4055,#4056,#4057,#4058,#4059,#4060,
#4061,#4062,#4063,#4064,#4065,#4066,#4067,#4068,#4069,#4070,#4071,#4072,
#4073,#4074,#4075,#4076,#4077,#4078,#4079,#4080,#4081,#4082,#4083,#4084,
#4085,#4086,#4087,#4088,#4089,#4090,#4091,#4092,#4093,#4094,#4095,#4096,
#4097,#4098,#4099,#4100,#4101,#4102,#4103,#4104,#4105,#4106,#4107,#4108,
#4109,#4110,#4111,#4112,#4113,#4114,#4115,#4116,#4117,#4118,#4119,#4120,
#4121,#4122,#4123,#4124,#4125,#4126,#4127,#4128,#4129,#4130,#4131,#4132,
#4133,#4134,#4135,#4136,#4137,#4138,#4139,#4140,#4141,#4142,#4143,#4144,
#4145,#4146,#4147,#4148,#4149,#4150,#4151,#4152,#4153,#4154,#4155,#4156,
#4157,#4158,#4159,#4160,#4161,#4162,#4163,#4164,#4165,#4166,#4167,#4168,
#4169,#4170,#4171,#4172,#4173,#4174,#4175,#4176,#4177,#4178,#4179,#4180,
#4181,#4182,#4183,#4184,#4185,#4186,#4187,#4188,#4189,#4190,#4191,#4192,
#4193,#4194,#4195,#4196,#4197,#4198,#4199,#4200,#4201,#4202,#4203,#4204,
#4205,#4206,#4207,#4208,#4209,#4210,#4211,#4212,#4213,#4214,#4215,#4216,
#4217,#4218,#4219,#4220,#4221,#4222,#4223,#4224,#4225,#4226,#4227,#4228,
#4229,#4230,#4231,#4232,#4233,#4234,#4235,#4236,#4237,#4238,#4239,#4240,
#4241,#4242,#4243,#4244,#4245,#4246,#4247,#4248,#4249,#4250,#4251,#4252,
#4253,#4254,#4255,#4256,#4257,#4258,#4259,#4260,#4261,#4262,#4263,#4264,
#4265,#4266,#4267,#4268,#4269,#4270,#4271,#4272,#4273,#4274,#4275,#4276,
#4277,#4278,#4279,#4280,#4281,#4282,#4283,#4284,#4285,#4286,#4287,#4288,
#4289,#4290,#4291,#4292,#4293,#4294,#4295),.UNSPECIFIED.,.F.,.F.,(4,3,3,
3,3,3,3,3,3,3,3,3,3,3,3,3,3,3,3,3,3,3,3,3,3,3,3,3,3,3,3,3,3,3,3,3,3,3,3,
3,3,3,3,3,3,3,3,3,3,3,3,3,3,3,3,3,3,3,3,3,3,3,3,3,3,3,3,3,3,3,3,3,3,3,3,
3,3,3,3,3,3,3,3,3,3,3,3,3,3,3,3,3,3,3,3,3,3,3,3,3,3,3,3,3,3,3,3,3,3,3,3,
3,3,3,3,3,3,3,3,3,3,3,3,3,3,3,3,3,4),(1.0000001042787E-6,0.0014871514523892,
0.0749567234267537,0.150089270788223,0.172088117470375,0.241130573114261,
0.312711766240772,0.343094857711695,0.381951662220986,0.421803865009944,
0.428901758240627,0.487519881652639,0.514134072896966,0.582840219819151,
0.657390551246057,0.737159327871297,0.831988683331776,0.852127431697674,
0.930562309987346,1.01139670060428,1.02773758699043,1.09799569327158,1.17527352760952,
1.23343415291206,1.25440919300555,1.25852070377139,1.30827982182686,1.36078487138267,
1.41569393131549,1.44625277535225,1.45683103644174,1.46757702369143,1.71074240249359,
1.9046354359037,2.15693173732147,2.4137324042945,2.66821353221044,2.88528820091008,
3.06961454817592,3.31666055499289,3.48038126011738,3.76387952993356,3.9660510033563,
3.99419905100257,4.00387960603785,4.17190313859031,4.47424018327161,4.5876165750271,
4.60600176545457,4.61648429138331,4.81078750052133,5.05617977077072,5.3812513173155,
5.6262534145718,5.84324989753007,6.03270067111654,6.21030165738215,6.38464570243243,
6.53909882881487,6.55898974748272,6.65552179344928,6.67007122930517,6.80699364566742,
6.9441380090924,7.08360518962895,7.23195205145568,7.33124611521517,7.49685632337973,
7.71469057821715,7.90521396436979,7.97306427912083,8.1326038530189,8.26595178400231,
8.39354231526298,8.5151857419584,8.6112225747131,8.67478294951946,8.69472463683432,
8.77994976234092,8.84186629348611,8.89672828572145,8.9515902779568,9.00448857161819,
9.05627744790037,9.10651371084493,9.11661034222362,9.14263302563896,9.15595525428157,
9.17603250358564,9.19697882034037,9.22071837731693,9.24114544445277,9.2872949501813,
9.31590918197957,9.3419598214356,9.36552499840417,9.37905935500493,9.42076096929037,
9.45178040154512,9.46246258357582,9.47817570718829,9.4936471631625,9.50905917788915,
9.52459264913576,9.54063041470408,9.54655850428292,9.56417707996487,9.58322181605694,
9.60106013585175,9.62444511738643,9.64813998687783,9.66423486245875,9.6919586017109,
9.72029263474653,9.72833972832233,9.75167849681345,9.77575531649194,9.79214986652168,
9.82904279829337,9.86641260150116,9.90467666556498,9.93420348302458,9.97272818736647,
10.0146788654693,10.0614145694852,10.0971799068754,10.2459044783698,10.2612321226266,
10.6513279635848),.UNSPECIFIED.);
#102=B_SPLINE_CURVE_WITH_KNOTS('',3,(#4305,#4306,#4307,#4308,#4309,#4310,
#4311,#4312,#4313,#4314,#4315,#4316,#4317,#4318,#4319,#4320,#4321,#4322,
#4323,#4324),.UNSPECIFIED.,.F.,.F.,(4,2,2,2,2,2,2,2,2,4),(9.9999998042934E-7,
0.000855968525488541,0.00182994379593221,0.00396192280934848,0.0107018008494555,
0.093963121684891,0.228860984301384,0.24733539739969,0.253328089464202,
0.258418228284023),.UNSPECIFIED.);
#103=B_SPLINE_CURVE_WITH_KNOTS('',3,(#4610,#4611,#4612,#4613,#4614,#4615,
#4616,#4617,#4618,#4619,#4620,#4621,#4622,#4623,#4624,#4625,#4626,#4627,
#4628,#4629,#4630,#4631,#4632,#4633,#4634,#4635,#4636,#4637,#4638,#4639,
#4640,#4641,#4642,#4643,#4644,#4645,#4646,#4647,#4648,#4649,#4650,#4651,
#4652,#4653,#4654,#4655,#4656,#4657,#4658,#4659,#4660,#4661,#4662,#4663,
#4664,#4665),.UNSPECIFIED.,.F.,.F.,(4,2,2,2,2,1,2,2,2,2,2,2,2,2,2,2,2,2,
2,2,2,2,2,1,2,2,2,2,4),(1.76202838341362E-9,0.00152946839585409,0.00573422822705338,
0.00994072554036124,0.0183588914643831,0.0352156178566175,0.0520989766057049,
0.0859428491008545,0.153919387862698,0.222241646761829,0.256517065813169,
0.290860192348371,0.35972332278199,0.4287774185551,0.497967334131587,0.571128173595134,
0.636528988048645,0.709831201875327,0.774953293421917,0.843972576608793,
0.878409790177993,0.91278972931851,0.947105790641693,0.964237837412799,
0.981351495675405,0.989901182362907,0.994174197253835,0.998445976951636,
0.999999997793755),.UNSPECIFIED.);
#104=B_SPLINE_CURVE_WITH_KNOTS('',2,(#4668,#4669,#4670),.UNSPECIFIED.,.F.,
 .F.,(3,3),(0.,1.),.UNSPECIFIED.);
#105=B_SPLINE_CURVE_WITH_KNOTS('',3,(#4684,#4685,#4686,#4687,#4688,#4689,
#4690,#4691,#4692,#4693,#4694,#4695,#4696),.UNSPECIFIED.,.F.,.F.,(4,3,3,
3,4),(-0.197909908995898,-0.15516480831031,-0.111768121995836,-0.0989540665429965,
0.),.UNSPECIFIED.);
#106=B_SPLINE_CURVE_WITH_KNOTS('',3,(#4698,#4699,#4700,#4701,#4702),
 .UNSPECIFIED.,.F.,.F.,(4,1,4),(0.0298132943020683,0.494943232770503,1.),
 .UNSPECIFIED.);
#107=B_SPLINE_CURVE_WITH_KNOTS('',3,(#4705,#4706,#4707,#4708,#4709),
 .UNSPECIFIED.,.F.,.F.,(4,1,4),(0.,0.494943232770503,1.),.UNSPECIFIED.);
#108=B_SPLINE_CURVE_WITH_KNOTS('',3,(#4738,#4739,#4740,#4741,#4742,#4743,
#4744,#4745,#4746,#4747,#4748,#4749),.UNSPECIFIED.,.F.,.F.,(4,1,1,1,1,1,
1,1,1,4),(0.0654911701302355,0.0728325313021349,0.151642943092782,0.236641834545795,
0.351573197840935,0.540150564955284,0.71598472862448,0.797600110822501,
0.875509677594327,1.),.UNSPECIFIED.);
#109=B_SPLINE_CURVE_WITH_KNOTS('',3,(#4752,#4753,#4754,#4755,#4756,#4757,
#4758,#4759,#4760,#4761,#4762,#4763),.UNSPECIFIED.,.F.,.F.,(4,1,1,1,1,1,
1,1,1,4),(0.0654911701302355,0.0728325313021349,0.151642943092782,0.236641834545795,
0.351573197840935,0.540150564955284,0.71598472862448,0.797600110822501,
0.875509677594327,1.),.UNSPECIFIED.);
#110=B_SPLINE_CURVE_WITH_KNOTS('',2,(#4771,#4772,#4773),.UNSPECIFIED.,.F.,
 .F.,(3,3),(0.,1.),.UNSPECIFIED.);
#111=B_SPLINE_CURVE_WITH_KNOTS('',2,(#4776,#4777,#4778),.UNSPECIFIED.,.F.,
 .F.,(3,3),(0.,1.),.UNSPECIFIED.);
#112=B_SPLINE_CURVE_WITH_KNOTS('',3,(#4782,#4783,#4784,#4785,#4786,#4787),
 .UNSPECIFIED.,.F.,.F.,(4,2,4),(-0.229871652660954,-0.114908525875315,0.),
 .UNSPECIFIED.);
#113=B_SPLINE_CURVE_WITH_KNOTS('',3,(#4792,#4793,#4794,#4795,#4796,#4797,
#4798,#4799,#4800,#4801,#4802,#4803,#4804,#4805,#4806,#4807,#4808,#4809,
#4810,#4811,#4812,#4813,#4814,#4815,#4816,#4817,#4818,#4819,#4820,#4821,
#4822,#4823,#4824,#4825,#4826,#4827,#4828,#4829,#4830,#4831,#4832,#4833,
#4834,#4835,#4836,#4837,#4838,#4839,#4840,#4841,#4842,#4843,#4844,#4845,
#4846,#4847,#4848,#4849,#4850,#4851,#4852,#4853,#4854,#4855,#4856,#4857,
#4858),.UNSPECIFIED.,.F.,.F.,(4,3,3,3,3,3,3,3,3,3,3,3,3,3,3,3,3,3,3,3,3,
3,4),(-4.14191399419292,-4.12414475765899,-4.04926436109822,-3.89944091710028,
-3.74954461699361,-3.59958832872791,-3.29954750710329,-2.90481294303335,
-2.69931657063712,-2.30568273196656,-2.09957968336527,-2.07307122857376,
-2.04569728092775,-1.79983587858531,-1.49976903624527,-1.19950941255717,
-1.0493493530693,-0.899191607974707,-0.598950483849536,-0.298920557742038,
-0.149026588716908,-0.0741171167945361,-1.00000000280431E-6),
 .UNSPECIFIED.);
#114=B_SPLINE_CURVE_WITH_KNOTS('',3,(#5044,#5045,#5046,#5047),
 .UNSPECIFIED.,.F.,.F.,(4,4),(0.,0.963009819411559),.UNSPECIFIED.);
#115=B_SPLINE_CURVE_WITH_KNOTS('',3,(#5049,#5050,#5051,#5052,#5053,#5054,
#5055),.UNSPECIFIED.,.F.,.F.,(4,3,4),(-0.194536582159801,-0.0969214136710641,
0.),.UNSPECIFIED.);
#116=B_SPLINE_CURVE_WITH_KNOTS('',3,(#5059,#5060,#5061,#5062),
 .UNSPECIFIED.,.F.,.F.,(4,4),(0.,1.),.UNSPECIFIED.);
#117=B_SPLINE_CURVE_WITH_KNOTS('',3,(#5071,#5072,#5073,#5074,#5075,#5076,
#5077,#5078,#5079,#5080,#5081,#5082,#5083,#5084,#5085,#5086,#5087,#5088,
#5089,#5090,#5091,#5092,#5093,#5094,#5095),.UNSPECIFIED.,.F.,.F.,(4,3,3,
3,3,3,3,3,4),(-4.76083539582986,-4.44733911607309,-4.152057580002,-3.01724680527447,
-2.29831043152851,-1.33769412810892,-0.608765253834458,-0.313488116787147,
0.),.UNSPECIFIED.);
#118=B_SPLINE_CURVE_WITH_KNOTS('',3,(#5131,#5132,#5133,#5134,#5135,#5136,
#5137,#5138,#5139,#5140,#5141,#5142,#5143,#5144,#5145),.UNSPECIFIED.,.F.,
 .F.,(4,1,1,1,1,1,1,1,1,1,1,1,4),(0.,0.157038713621339,0.211241890914945,
0.295200207692272,0.373845032775918,0.419097916699999,0.461946250305228,
0.500883855221145,0.554258304196424,0.580360336370224,0.654376236660092,
0.774520045331176,1.),.UNSPECIFIED.);
#119=B_SPLINE_CURVE_WITH_KNOTS('',3,(#5149,#5150,#5151,#5152,#5153,#5154,
#5155,#5156,#5157,#5158,#5159,#5160,#5161,#5162,#5163),.UNSPECIFIED.,.F.,
 .F.,(4,1,1,1,1,1,1,1,1,1,1,1,4),(0.,0.157038713621339,0.211241890914945,
0.295200207692272,0.373845032775918,0.419097916699999,0.461946250305228,
0.500883855221145,0.554258304196424,0.580360336370224,0.654376236660092,
0.774520045331176,1.),.UNSPECIFIED.);
#120=B_SPLINE_CURVE_WITH_KNOTS('',3,(#5178,#5179,#5180,#5181,#5182,#5183),
 .UNSPECIFIED.,.F.,.F.,(4,2,4),(1.00000017285152E-6,4.02327180930654,8.26259118342642),
 .UNSPECIFIED.);
#121=B_SPLINE_CURVE_WITH_KNOTS('',3,(#5366,#5367,#5368,#5369,#5370,#5371,
#5372,#5373,#5374,#5375,#5376,#5377),.UNSPECIFIED.,.F.,.F.,(4,2,2,2,2,4),
(0.727251200985696,0.761344800862484,0.795438400739272,0.863625600492848,
0.931812800246424,0.997527670949997),.UNSPECIFIED.);
#122=B_SPLINE_CURVE_WITH_KNOTS('',3,(#5382,#5383,#5384,#5385,#5386,#5387,
#5388,#5389,#5390,#5391,#5392,#5393),.UNSPECIFIED.,.F.,.F.,(4,2,2,2,2,4),
(0.727251200985696,0.761344800862484,0.795438400739272,0.863625600492848,
0.931812800246424,1.),.UNSPECIFIED.);
#123=B_SPLINE_CURVE_WITH_KNOTS('',3,(#5676,#5677,#5678,#5679,#5680,#5681,
#5682,#5683,#5684,#5685,#5686,#5687,#5688,#5689,#5690,#5691,#5692,#5693,
#5694,#5695,#5696,#5697,#5698,#5699),.UNSPECIFIED.,.F.,.F.,(4,2,2,2,2,2,
2,2,2,2,2,4),(-0.0558533803830892,-0.0554200089354374,-0.0551962315488395,
-0.0547444182972245,-0.0538796394902973,-0.0521571275021974,-0.0487120777231514,
-0.041906416333374,-0.0288960116062435,-0.0178108635562527,-0.00795577739213343,
-1.45747604985572E-5),.UNSPECIFIED.);
#124=B_SPLINE_CURVE_WITH_KNOTS('',3,(#5701,#5702,#5703,#5704,#5705,#5706,
#5707,#5708,#5709,#5710,#5711,#5712,#5713,#5714,#5715,#5716,#5717,#5718,
#5719,#5720,#5721,#5722,#5723,#5724,#5725,#5726,#5727,#5728,#5729,#5730,
#5731,#5732,#5733,#5734,#5735,#5736,#5737,#5738,#5739,#5740,#5741,#5742,
#5743,#5744,#5745,#5746),.UNSPECIFIED.,.F.,.F.,(4,2,2,2,2,2,2,2,2,2,2,2,
2,2,2,2,2,2,2,2,2,2,4),(0.00725097420749211,0.0166371724554133,0.0261818111535564,
0.0359748592316744,0.0437517296050677,0.0875034592101353,0.131255188815203,
0.175006918420271,0.196882783222805,0.218758648025338,0.262510377630406,
0.350013836840541,0.418185084306466,0.48635633177239,0.554527579238314,
0.622698826704238,0.669861473366208,0.717024120028179,0.81134941335212,
0.85851206001409,0.905674706676061,0.952837353338031,1.),.UNSPECIFIED.);
#125=B_SPLINE_CURVE_WITH_KNOTS('',3,(#5750,#5751,#5752,#5753,#5754,#5755,
#5756,#5757,#5758,#5759,#5760,#5761,#5762,#5763,#5764,#5765,#5766,#5767,
#5768,#5769,#5770,#5771,#5772,#5773,#5774,#5775,#5776,#5777,#5778,#5779,
#5780,#5781,#5782,#5783,#5784,#5785,#5786,#5787,#5788,#5789),
 .UNSPECIFIED.,.F.,.F.,(4,2,2,2,2,2,2,2,2,2,2,2,2,2,2,2,2,2,2,4),(0.,0.0437517296050676,
0.0875034592101352,0.131255188815203,0.17500691842027,0.196882783222804,
0.218758648025338,0.262510377630406,0.350013836840541,0.418185084306465,
0.486356331772389,0.554527579238313,0.622698826704237,0.669861473366207,
0.717024120028178,0.811349413352118,0.858512060014089,0.905674706676059,
0.95283735333803,1.),.UNSPECIFIED.);
#126=B_SPLINE_CURVE_WITH_KNOTS('',3,(#7920,#7921,#7922,#7923,#7924,#7925,
#7926,#7927,#7928,#7929,#7930,#7931,#7932,#7933,#7934,#7935,#7936,#7937,
#7938,#7939,#7940,#7941,#7942,#7943,#7944,#7945,#7946,#7947,#7948,#7949,
#7950,#7951,#7952,#7953,#7954,#7955,#7956,#7957,#7958,#7959,#7960,#7961,
#7962,#7963,#7964,#7965,#7966,#7967,#7968,#7969,#7970,#7971,#7972,#7973,
#7974,#7975,#7976,#7977,#7978,#7979,#7980,#7981,#7982,#7983,#7984,#7985,
#7986,#7987,#7988,#7989,#7990,#7991,#7992,#7993,#7994,#7995,#7996,#7997,
#7998,#7999,#8000,#8001,#8002,#8003,#8004,#8005,#8006,#8007,#8008,#8009,
#8010,#8011,#8012,#8013,#8014,#8015,#8016,#8017,#8018,#8019,#8020,#8021,
#8022,#8023,#8024,#8025,#8026,#8027,#8028,#8029,#8030,#8031,#8032,#8033,
#8034,#8035,#8036,#8037,#8038,#8039,#8040,#8041,#8042,#8043,#8044,#8045,
#8046,#8047,#8048,#8049,#8050,#8051,#8052,#8053,#8054,#8055,#8056,#8057,
#8058,#8059,#8060,#8061,#8062,#8063,#8064,#8065,#8066,#8067,#8068,#8069,
#8070,#8071,#8072,#8073,#8074,#8075,#8076,#8077,#8078,#8079,#8080,#8081,
#8082,#8083,#8084,#8085,#8086,#8087,#8088,#8089,#8090,#8091,#8092,#8093,
#8094,#8095,#8096,#8097,#8098,#8099,#8100,#8101,#8102,#8103,#8104,#8105,
#8106,#8107,#8108,#8109,#8110,#8111,#8112,#8113,#8114,#8115,#8116,#8117,
#8118,#8119,#8120,#8121,#8122,#8123,#8124,#8125,#8126,#8127,#8128,#8129,
#8130,#8131,#8132,#8133,#8134,#8135,#8136,#8137,#8138,#8139,#8140,#8141,
#8142,#8143,#8144,#8145,#8146,#8147,#8148,#8149,#8150,#8151,#8152,#8153,
#8154,#8155,#8156,#8157,#8158,#8159,#8160,#8161,#8162,#8163,#8164,#8165,
#8166,#8167,#8168,#8169,#8170,#8171,#8172,#8173,#8174,#8175,#8176,#8177,
#8178,#8179,#8180,#8181,#8182,#8183,#8184,#8185,#8186,#8187,#8188,#8189,
#8190,#8191,#8192,#8193,#8194,#8195,#8196,#8197,#8198,#8199,#8200,#8201,
#8202,#8203,#8204,#8205,#8206,#8207,#8208,#8209,#8210,#8211,#8212,#8213,
#8214,#8215,#8216,#8217,#8218,#8219,#8220,#8221,#8222,#8223,#8224,#8225,
#8226,#8227,#8228,#8229,#8230,#8231,#8232,#8233,#8234,#8235,#8236,#8237,
#8238,#8239,#8240,#8241,#8242,#8243,#8244,#8245,#8246,#8247,#8248,#8249,
#8250,#8251,#8252,#8253,#8254,#8255,#8256,#8257,#8258,#8259,#8260,#8261,
#8262,#8263,#8264,#8265,#8266,#8267,#8268,#8269,#8270,#8271,#8272,#8273,
#8274,#8275,#8276,#8277,#8278,#8279,#8280,#8281,#8282,#8283,#8284,#8285,
#8286,#8287,#8288,#8289,#8290,#8291,#8292,#8293,#8294,#8295,#8296,#8297,
#8298,#8299,#8300,#8301,#8302,#8303,#8304,#8305,#8306,#8307,#8308,#8309,
#8310,#8311,#8312,#8313,#8314,#8315,#8316,#8317,#8318,#8319,#8320,#8321,
#8322,#8323,#8324,#8325,#8326,#8327,#8328,#8329,#8330,#8331,#8332,#8333,
#8334,#8335,#8336,#8337,#8338,#8339,#8340,#8341,#8342,#8343,#8344,#8345,
#8346,#8347,#8348,#8349,#8350,#8351,#8352,#8353,#8354,#8355,#8356,#8357,
#8358,#8359,#8360,#8361,#8362,#8363,#8364,#8365,#8366,#8367,#8368,#8369,
#8370,#8371,#8372,#8373,#8374,#8375,#8376,#8377,#8378,#8379,#8380,#8381,
#8382,#8383,#8384,#8385,#8386,#8387,#8388,#8389,#8390,#8391,#8392,#8393,
#8394,#8395,#8396,#8397,#8398,#8399,#8400,#8401,#8402,#8403,#8404,#8405,
#8406,#8407,#8408,#8409,#8410,#8411,#8412,#8413,#8414,#8415,#8416,#8417,
#8418,#8419,#8420,#8421,#8422,#8423,#8424,#8425,#8426,#8427,#8428,#8429,
#8430,#8431,#8432,#8433,#8434,#8435,#8436,#8437,#8438,#8439,#8440,#8441,
#8442,#8443,#8444,#8445,#8446,#8447,#8448,#8449,#8450,#8451,#8452,#8453,
#8454,#8455,#8456,#8457,#8458,#8459,#8460,#8461,#8462,#8463,#8464,#8465,
#8466,#8467,#8468,#8469,#8470,#8471,#8472,#8473,#8474,#8475,#8476,#8477,
#8478,#8479,#8480,#8481,#8482,#8483,#8484,#8485,#8486,#8487,#8488,#8489,
#8490,#8491,#8492,#8493,#8494,#8495,#8496,#8497,#8498,#8499,#8500,#8501,
#8502,#8503,#8504,#8505,#8506,#8507,#8508,#8509,#8510,#8511,#8512,#8513,
#8514,#8515,#8516,#8517,#8518,#8519,#8520,#8521,#8522,#8523,#8524,#8525,
#8526,#8527,#8528,#8529,#8530,#8531,#8532,#8533,#8534,#8535,#8536,#8537,
#8538,#8539,#8540,#8541,#8542,#8543,#8544,#8545,#8546,#8547,#8548,#8549,
#8550,#8551,#8552,#8553,#8554,#8555,#8556,#8557,#8558,#8559,#8560,#8561,
#8562,#8563,#8564,#8565,#8566,#8567,#8568,#8569,#8570,#8571,#8572,#8573,
#8574,#8575,#8576,#8577,#8578,#8579,#8580,#8581,#8582,#8583,#8584,#8585,
#8586,#8587,#8588,#8589,#8590,#8591,#8592,#8593,#8594,#8595,#8596,#8597,
#8598,#8599,#8600,#8601,#8602,#8603,#8604,#8605,#8606,#8607,#8608,#8609,
#8610,#8611,#8612,#8613,#8614,#8615,#8616,#8617,#8618,#8619,#8620,#8621,
#8622,#8623,#8624,#8625,#8626,#8627,#8628,#8629,#8630,#8631,#8632,#8633,
#8634,#8635,#8636,#8637,#8638,#8639,#8640,#8641,#8642,#8643,#8644,#8645,
#8646,#8647,#8648,#8649,#8650,#8651,#8652,#8653,#8654,#8655,#8656,#8657,
#8658,#8659,#8660,#8661,#8662,#8663,#8664,#8665,#8666,#8667,#8668,#8669,
#8670,#8671,#8672,#8673,#8674,#8675,#8676,#8677,#8678,#8679,#8680,#8681,
#8682,#8683,#8684,#8685,#8686,#8687,#8688,#8689,#8690,#8691,#8692,#8693,
#8694,#8695,#8696,#8697,#8698,#8699,#8700,#8701,#8702,#8703,#8704,#8705,
#8706,#8707,#8708,#8709,#8710,#8711,#8712,#8713,#8714,#8715,#8716,#8717,
#8718,#8719,#8720,#8721,#8722,#8723,#8724,#8725,#8726,#8727,#8728,#8729,
#8730,#8731,#8732,#8733,#8734,#8735,#8736,#8737,#8738,#8739,#8740,#8741,
#8742,#8743,#8744,#8745,#8746,#8747,#8748,#8749,#8750,#8751,#8752,#8753,
#8754,#8755,#8756,#8757,#8758,#8759,#8760,#8761,#8762,#8763,#8764,#8765,
#8766,#8767,#8768,#8769,#8770,#8771,#8772,#8773,#8774,#8775,#8776,#8777,
#8778,#8779,#8780,#8781,#8782,#8783,#8784,#8785,#8786,#8787,#8788,#8789,
#8790,#8791,#8792,#8793,#8794,#8795,#8796,#8797,#8798,#8799,#8800,#8801,
#8802,#8803,#8804,#8805,#8806,#8807,#8808,#8809,#8810,#8811,#8812,#8813,
#8814,#8815,#8816,#8817,#8818,#8819,#8820,#8821,#8822,#8823,#8824,#8825,
#8826,#8827,#8828,#8829,#8830,#8831,#8832,#8833,#8834,#8835,#8836,#8837,
#8838,#8839,#8840,#8841,#8842,#8843,#8844,#8845,#8846,#8847,#8848,#8849,
#8850,#8851,#8852,#8853,#8854,#8855,#8856,#8857,#8858,#8859,#8860,#8861,
#8862,#8863,#8864,#8865,#8866,#8867,#8868,#8869,#8870,#8871,#8872,#8873,
#8874,#8875,#8876,#8877,#8878,#8879,#8880,#8881,#8882,#8883,#8884,#8885,
#8886,#8887,#8888,#8889,#8890,#8891,#8892,#8893,#8894,#8895,#8896,#8897,
#8898,#8899,#8900,#8901,#8902,#8903,#8904,#8905,#8906,#8907,#8908,#8909,
#8910,#8911,#8912,#8913,#8914,#8915,#8916,#8917,#8918,#8919,#8920,#8921,
#8922,#8923,#8924,#8925,#8926,#8927,#8928,#8929,#8930,#8931,#8932,#8933,
#8934,#8935,#8936,#8937,#8938,#8939,#8940,#8941,#8942,#8943,#8944,#8945,
#8946,#8947,#8948,#8949,#8950,#8951,#8952,#8953,#8954,#8955,#8956,#8957,
#8958,#8959,#8960,#8961,#8962,#8963,#8964,#8965,#8966,#8967,#8968,#8969,
#8970,#8971,#8972,#8973,#8974,#8975,#8976,#8977,#8978,#8979,#8980,#8981,
#8982,#8983,#8984,#8985,#8986,#8987,#8988,#8989,#8990,#8991,#8992,#8993,
#8994,#8995,#8996,#8997,#8998,#8999,#9000,#9001,#9002,#9003,#9004,#9005,
#9006,#9007,#9008,#9009,#9010,#9011,#9012,#9013,#9014,#9015,#9016,#9017,
#9018,#9019,#9020,#9021,#9022,#9023,#9024,#9025,#9026,#9027,#9028,#9029,
#9030,#9031,#9032,#9033,#9034,#9035,#9036,#9037,#9038,#9039,#9040,#9041,
#9042,#9043,#9044,#9045,#9046,#9047,#9048,#9049,#9050,#9051,#9052,#9053,
#9054,#9055,#9056,#9057,#9058,#9059,#9060,#9061,#9062,#9063,#9064,#9065,
#9066,#9067,#9068,#9069,#9070,#9071,#9072,#9073,#9074,#9075,#9076,#9077,
#9078,#9079,#9080,#9081,#9082,#9083,#9084,#9085,#9086,#9087,#9088,#9089,
#9090,#9091,#9092,#9093,#9094,#9095,#9096,#9097,#9098,#9099,#9100,#9101,
#9102,#9103,#9104,#9105,#9106,#9107,#9108,#9109,#9110,#9111,#9112,#9113,
#9114,#9115,#9116,#9117,#9118,#9119,#9120,#9121,#9122,#9123,#9124,#9125,
#9126,#9127,#9128,#9129,#9130,#9131,#9132,#9133,#9134,#9135,#9136,#9137,
#9138,#9139,#9140,#9141,#9142,#9143,#9144,#9145,#9146,#9147,#9148,#9149,
#9150,#9151,#9152,#9153,#9154,#9155,#9156,#9157,#9158,#9159,#9160,#9161,
#9162,#9163,#9164,#9165,#9166,#9167,#9168,#9169,#9170,#9171,#9172,#9173,
#9174,#9175,#9176,#9177,#9178,#9179,#9180,#9181,#9182,#9183,#9184,#9185,
#9186,#9187,#9188,#9189,#9190,#9191,#9192,#9193,#9194,#9195,#9196,#9197,
#9198,#9199,#9200,#9201,#9202,#9203,#9204,#9205,#9206,#9207,#9208,#9209,
#9210,#9211,#9212,#9213,#9214,#9215,#9216,#9217,#9218,#9219,#9220,#9221,
#9222,#9223,#9224,#9225,#9226,#9227,#9228,#9229,#9230,#9231,#9232,#9233,
#9234,#9235,#9236,#9237,#9238,#9239,#9240,#9241,#9242,#9243,#9244,#9245,
#9246,#9247,#9248,#9249,#9250,#9251,#9252,#9253,#9254,#9255,#9256,#9257,
#9258,#9259,#9260,#9261,#9262,#9263,#9264,#9265,#9266,#9267,#9268,#9269,
#9270,#9271,#9272,#9273,#9274,#9275,#9276,#9277,#9278,#9279,#9280,#9281,
#9282,#9283,#9284,#9285,#9286,#9287,#9288,#9289,#9290,#9291,#9292,#9293,
#9294,#9295,#9296,#9297,#9298,#9299,#9300,#9301,#9302,#9303,#9304,#9305,
#9306,#9307,#9308,#9309,#9310,#9311,#9312,#9313,#9314,#9315,#9316,#9317,
#9318,#9319,#9320,#9321,#9322,#9323,#9324,#9325,#9326,#9327,#9328,#9329,
#9330,#9331,#9332,#9333,#9334,#9335,#9336,#9337,#9338,#9339,#9340,#9341,
#9342,#9343,#9344,#9345,#9346,#9347,#9348,#9349,#9350,#9351,#9352,#9353,
#9354,#9355,#9356,#9357,#9358,#9359,#9360,#9361,#9362,#9363,#9364,#9365,
#9366,#9367,#9368,#9369,#9370,#9371,#9372,#9373,#9374,#9375,#9376,#9377,
#9378,#9379,#9380,#9381,#9382,#9383,#9384,#9385,#9386,#9387,#9388,#9389,
#9390,#9391,#9392,#9393,#9394,#9395,#9396,#9397,#9398,#9399,#9400,#9401,
#9402,#9403,#9404,#9405,#9406,#9407,#9408,#9409,#9410,#9411,#9412,#9413,
#9414,#9415,#9416,#9417,#9418,#9419,#9420,#9421,#9422,#9423,#9424,#9425,
#9426,#9427,#9428,#9429,#9430,#9431,#9432,#9433,#9434,#9435,#9436,#9437,
#9438,#9439,#9440,#9441,#9442,#9443,#9444,#9445,#9446,#9447,#9448,#9449,
#9450,#9451,#9452,#9453,#9454,#9455,#9456,#9457,#9458,#9459,#9460,#9461,
#9462,#9463,#9464,#9465,#9466,#9467,#9468,#9469,#9470,#9471,#9472,#9473,
#9474,#9475,#9476,#9477,#9478,#9479,#9480,#9481,#9482,#9483,#9484,#9485,
#9486,#9487,#9488,#9489,#9490,#9491,#9492,#9493,#9494,#9495,#9496,#9497,
#9498,#9499,#9500,#9501,#9502,#9503,#9504,#9505,#9506,#9507,#9508,#9509,
#9510,#9511,#9512,#9513,#9514,#9515,#9516,#9517,#9518,#9519,#9520,#9521,
#9522,#9523,#9524,#9525,#9526,#9527,#9528,#9529,#9530,#9531,#9532,#9533,
#9534,#9535,#9536,#9537,#9538,#9539,#9540,#9541,#9542,#9543,#9544,#9545,
#9546,#9547,#9548,#9549,#9550,#9551,#9552,#9553,#9554,#9555,#9556,#9557,
#9558,#9559,#9560,#9561,#9562,#9563,#9564,#9565,#9566,#9567,#9568,#9569,
#9570,#9571,#9572,#9573,#9574,#9575,#9576,#9577,#9578,#9579,#9580,#9581,
#9582,#9583,#9584,#9585,#9586,#9587,#9588,#9589,#9590,#9591,#9592,#9593,
#9594,#9595,#9596,#9597,#9598,#9599,#9600,#9601,#9602,#9603,#9604,#9605,
#9606,#9607,#9608,#9609,#9610,#9611,#9612,#9613,#9614,#9615,#9616,#9617,
#9618,#9619,#9620,#9621,#9622,#9623,#9624,#9625,#9626,#9627,#9628,#9629,
#9630,#9631,#9632,#9633,#9634,#9635,#9636,#9637,#9638,#9639,#9640,#9641,
#9642,#9643,#9644,#9645,#9646,#9647,#9648,#9649,#9650,#9651,#9652,#9653,
#9654,#9655,#9656,#9657,#9658,#9659,#9660,#9661,#9662,#9663,#9664,#9665,
#9666,#9667,#9668,#9669,#9670,#9671,#9672,#9673,#9674,#9675,#9676,#9677,
#9678,#9679,#9680,#9681,#9682,#9683,#9684,#9685,#9686,#9687,#9688,#9689,
#9690,#9691,#9692,#9693,#9694,#9695,#9696,#9697,#9698,#9699,#9700,#9701,
#9702,#9703,#9704,#9705,#9706,#9707,#9708,#9709,#9710,#9711,#9712,#9713,
#9714,#9715,#9716,#9717,#9718,#9719,#9720,#9721,#9722,#9723,#9724,#9725,
#9726,#9727,#9728,#9729,#9730,#9731,#9732,#9733,#9734,#9735,#9736,#9737,
#9738,#9739,#9740,#9741,#9742,#9743,#9744,#9745,#9746,#9747,#9748,#9749,
#9750,#9751,#9752,#9753,#9754,#9755,#9756,#9757,#9758,#9759,#9760,#9761,
#9762,#9763,#9764,#9765,#9766,#9767,#9768,#9769,#9770,#9771,#9772,#9773,
#9774,#9775,#9776,#9777,#9778,#9779,#9780,#9781,#9782,#9783,#9784,#9785,
#9786,#9787,#9788,#9789,#9790,#9791,#9792,#9793,#9794,#9795,#9796,#9797,
#9798,#9799,#9800,#9801,#9802,#9803,#9804,#9805,#9806,#9807,#9808,#9809,
#9810,#9811,#9812,#9813,#9814,#9815,#9816,#9817,#9818,#9819,#9820,#9821,
#9822,#9823,#9824,#9825,#9826,#9827,#9828,#9829,#9830,#9831,#9832,#9833,
#9834,#9835,#9836,#9837,#9838,#9839,#9840,#9841,#9842,#9843,#9844,#9845,
#9846,#9847,#9848,#9849,#9850,#9851,#9852,#9853,#9854,#9855,#9856,#9857,
#9858,#9859,#9860,#9861,#9862,#9863,#9864,#9865,#9866,#9867,#9868,#9869,
#9870,#9871,#9872,#9873,#9874,#9875,#9876,#9877,#9878,#9879,#9880,#9881,
#9882,#9883,#9884,#9885,#9886,#9887,#9888,#9889,#9890,#9891,#9892,#9893,
#9894,#9895,#9896,#9897,#9898,#9899,#9900,#9901,#9902,#9903,#9904,#9905,
#9906,#9907,#9908,#9909,#9910,#9911,#9912,#9913,#9914,#9915,#9916,#9917,
#9918,#9919,#9920,#9921,#9922,#9923,#9924,#9925,#9926,#9927,#9928,#9929,
#9930,#9931,#9932,#9933),.UNSPECIFIED.,.F.,.F.,(4,3,3,3,3,3,3,3,3,3,3,3,
3,3,3,3,3,3,3,3,3,3,3,3,3,3,3,3,3,3,3,3,3,3,3,3,3,3,3,3,3,3,3,3,3,3,3,3,
3,3,3,3,3,3,3,3,3,3,3,3,3,3,3,3,3,3,3,3,3,3,3,3,3,3,3,3,3,3,3,3,3,3,3,3,
3,3,3,3,3,3,3,3,3,3,3,3,3,3,3,3,3,3,3,3,3,3,3,3,3,3,3,3,3,3,3,3,3,3,3,3,
3,3,3,3,3,3,3,3,3,3,3,3,3,3,3,3,3,3,3,3,3,3,3,3,3,3,3,3,3,3,3,3,3,3,3,3,
3,3,3,3,3,3,3,3,3,3,3,3,3,3,3,3,3,3,3,3,3,3,3,3,3,3,3,3,3,3,3,3,3,3,3,3,
3,3,3,3,3,3,3,3,3,3,3,3,3,3,3,3,3,3,3,3,3,3,3,3,3,3,3,3,3,3,3,3,3,3,3,3,
3,3,3,3,3,3,3,3,3,3,3,3,3,3,3,3,3,3,3,3,3,3,3,3,3,3,3,3,3,3,3,3,3,3,3,3,
3,3,3,3,3,3,3,3,3,3,3,3,3,3,3,3,3,3,3,3,3,3,3,3,3,3,3,3,3,3,3,3,3,3,3,3,
3,3,3,3,3,3,3,3,3,3,3,3,3,3,3,3,3,3,3,3,3,3,3,3,3,3,3,3,3,3,3,3,3,3,3,3,
3,3,3,3,3,3,3,3,3,3,3,3,3,3,3,3,3,3,3,3,3,3,3,3,3,3,3,3,3,3,3,3,3,3,3,3,
3,3,3,3,3,3,3,3,3,3,3,3,3,3,3,3,3,3,3,3,3,3,3,3,3,3,3,3,3,3,3,3,3,3,3,3,
3,3,3,3,3,3,3,3,3,3,3,3,3,3,3,3,3,3,3,3,3,3,3,3,3,3,3,3,3,3,3,3,3,3,3,3,
3,3,3,3,3,3,3,3,3,3,3,3,3,3,3,3,3,3,3,3,3,3,3,3,3,3,3,3,3,3,3,3,3,3,3,3,
3,3,3,3,3,3,3,3,3,3,3,3,3,3,3,3,3,3,3,3,3,3,3,3,3,3,3,3,3,3,3,3,3,3,3,3,
3,3,3,3,3,3,3,3,3,3,3,3,3,3,3,3,3,3,3,3,3,3,3,3,3,3,3,3,3,3,3,3,3,3,3,3,
3,3,3,3,3,3,3,3,3,3,3,3,3,3,3,3,3,3,3,3,3,3,3,3,3,3,3,3,3,3,3,3,3,3,3,3,
3,3,3,3,3,3,3,3,3,3,3,3,3,3,3,3,3,3,3,3,3,3,3,3,3,3,3,3,3,3,3,3,3,3,3,3,
3,3,3,3,3,3,3,3,3,3,3,3,3,3,3,3,3,3,3,3,3,3,3,3,3,3,3,3,3,3,3,3,3,3,3,3,
3,3,3,3,3,3,3,3,3,3,3,4),(0.00125565797610475,0.00293779707252473,0.00462005004901106,
0.00630132145657572,0.00798471684523592,0.00966590002453388,0.0104166666666667,
0.012100881513486,0.0137828211688803,0.0154854158976119,0.0171670252582823,
0.0188801126710445,0.0205932000838067,0.0208333333333333,0.022517548180085,
0.0241994878356134,0.0259020825643315,0.0275836919248216,0.0292967793376537,
0.0310098667504858,0.03125,0.0329342148472603,0.0346161545021281,0.0363187492308837,
0.0380003585915209,0.0397134460043357,0.0414265334171504,0.0416666666666667,
0.0433508815137824,0.0450328211690335,0.0467354158977296,0.0484170252579816,
0.0501301126708997,0.0518432000838178,0.0520833333333333,0.0537675481803484,
0.0554494878353327,0.0571520825641202,0.0588336919246883,0.0605467793375856,
0.0622598667504829,0.0625,0.064184214846777,0.0658661545020901,0.0675687492308563,
0.0692503585913632,0.0709634460042591,0.0726765334171549,0.0729166666666667,
0.0746008815139086,0.0762828211685875,0.0779854158973962,0.0796670252578115,
0.081380112670817,0.0830932000838225,0.0833333333333333,0.0850175481801576,
0.0866994878356449,0.0884020825643555,0.0900836919248141,0.0917967793376506,
0.0935098667504872,0.09375,0.0954342148471595,0.0971161545021867,0.0988187492309266,
0.100500358591525,0.102213446004336,0.103926533417146,0.104166666666667,
0.105850881513497,0.107532821168975,0.109235415897687,0.110917025258164,
0.112630112670993,0.114343200083822,0.114583333333333,0.116267548180165,
0.117949487835598,0.119652082564317,0.121333691924794,0.123046779337634,
0.124759866750474,0.125,0.126684214846945,0.128366154502066,0.130068749230835,
0.131750358591032,0.133463446004086,0.135176533417139,0.135416666666667,
0.137100881513744,0.138782821169231,0.140485415897875,0.142167025258217,
0.143880112671013,0.14559320008381,0.145833333333333,0.147517548180376,
0.149199487835436,0.150902082564201,0.152583691924607,0.154296779337552,
0.156009866750498,0.15625,0.157934214846695,0.159616154502591,0.161318749231229,
0.163000358591745,0.164713446004444,0.166426533417143,0.166666666666667,
0.168350881513626,0.170032821168768,0.17173541589753,0.173417025257758,
0.175130112670786,0.176843200083815,0.177083333333333,0.17876754818045,
0.180449487835452,0.182152082564211,0.183833691924545,0.185546779337517,
0.187259866750489,0.1875,0.189184214846864,0.190866154502186,0.192568749230926,
0.19425035859113,0.195963446004139,0.197676533417148,0.197916666666667,
0.199600881513898,0.201282821168701,0.202985415897484,0.204667025258033,
0.206380112670933,0.208093200083834,0.208333333333333,0.21001754818046,
0.211699487835182,0.213402082564005,0.215083691924369,0.216796779337423,
0.218509866750476,0.21875,0.220434214847214,0.222116154502313,0.223818749231029,
0.225500358591701,0.227213446004438,0.228926533417176,0.229166666666667,
0.230850881513923,0.232532821168741,0.234235415897509,0.235917025257756,
0.237630112670783,0.23934320008381,0.239583333333333,0.241267548180357,
0.242949487835833,0.244652082564497,0.246333691924975,0.248046779337732,
0.249759866750488,0.25,0.251684214846835,0.253366154502682,0.255068749231299,
0.256750358591701,0.258463446004426,0.26017653341715,0.260416666666667,
0.262100881513437,0.263782821168335,0.265485415897202,0.26716702525756,
0.268880112670682,0.270593200083804,0.270833333333333,0.272517548179882,
0.27419948783552,0.275902082564257,0.2775836919246,0.279296779337534,0.281009866750468,
0.28125,0.282934214846406,0.284616154502373,0.286318749231068,0.288000358591586,
0.289713446004369,0.291426533417152,0.291666666666667,0.293350881513846,
0.295032821168853,0.296735415897596,0.298417025257966,0.300130112670895,
0.301843200083824,0.302083333333333,0.303767548180358,0.30544948783509,
0.307152082563931,0.308833691924725,0.310546779337589,0.312259866750454,
0.3125,0.314184214846726,0.315866154501688,0.317568749230567,0.319250358591126,
0.320963446004165,0.322676533417204,0.322916666666667,0.32460088151406,
0.326282821168734,0.327985415897512,0.329667025257995,0.331380112670921,
0.333093200083847,0.333333333333333,0.335017548180048,0.336699487834948,
0.338402082563829,0.340083691924322,0.341796779337397,0.343509866750471,
0.34375,0.345434214847071,0.347116154502291,0.348818749231006,0.350500358591492,
0.352213446004321,0.35392653341715,0.354166666666667,0.35585088151403,0.357532821168803,
0.359235415897553,0.36091702525804,0.362630112670922,0.364343200083804,
0.364583333333333,0.36626754818007,0.36794948783571,0.369652082564395,0.371333691924692,
0.373046779337572,0.374759866750451,0.375,0.376684214846999,0.378366154502077,
0.380068749230849,0.3817503585914,0.383463446004282,0.385176533417163,0.385416666666667,
0.38710088928785,0.388782855752899,0.390545475148008,0.392227213127909,
0.393908936242942,0.395593200101389,0.395833333333333,0.397517548180182,
0.399199487835114,0.400902082563955,0.402583691924499,0.404296779337489,
0.40600986675048,0.40625,0.40793421484716,0.4096161545024,0.411318749231088,
0.413000358591541,0.414713446004348,0.416426533417155,0.416666666666667,
0.418350881513887,0.420032821169324,0.421735415897952,0.423417025258456,
0.425130112671146,0.426843200083836,0.427083333333333,0.428767548180366,
0.430449487835149,0.432152082563989,0.433833691924315,0.435546779337412,
0.437259866750508,0.4375,0.439184214846839,0.440866154501917,0.442568749230727,
0.444250358591221,0.445963446004191,0.44767653341716,0.447916666666667,
0.449600881513151,0.451282821169071,0.452985415897763,0.454667025258216,
0.456380112671027,0.458093200083838,0.458333333333333,0.460017548180184,
0.461699487835326,0.463402082564116,0.465083691924321,0.466796779337403,
0.468509866750486,0.46875,0.470434214846899,0.472116154502217,0.473818749230949,
0.475500358591599,0.477213446004371,0.478926533417144,0.479166666666667,
0.480850881514302,0.482532821168333,0.484235415897197,0.485917025257881,
0.487630112670835,0.489343200083788,0.489583333333333,0.491267548180153,
0.49294948783568,0.494652082564382,0.49633369192484,0.498046779337664,0.499759866750487,
0.5,0.501684214847251,0.503366154502004,0.505068749230785,0.506750358591275,
0.508463446004202,0.510176533417129,0.510416666666667,0.512100881513675,
0.513782821169851,0.515485415898353,0.517167025258938,0.518880112671398,
0.520593200083858,0.520833333333333,0.522517555953995,0.524199495600808,
0.525902088388242,0.527583697746963,0.529296782248755,0.531009866750547,
0.53125,0.532934214846679,0.534616154501946,0.536318749230739,0.53800035859119,
0.539713446004154,0.541426533417118,0.541666666666667,0.543350881514246,
0.545032821169243,0.546735415897896,0.548417025258523,0.55013011267119,
0.551843200083857,0.552083333333333,0.553767548180513,0.55544948783573,
0.557152082564415,0.558833691924724,0.560546779337596,0.562259866750468,
0.5625,0.564184214846736,0.5658661545017,0.567568749230563,0.569250358591102,
0.570963446004127,0.572676533417152,0.572916666666667,0.574600881513633,
0.576282821168363,0.57798541589723,0.579667025257621,0.581380112670727,
0.583093200083833,0.583333333333333,0.585017548180279,0.586699487835742,
0.588402082564422,0.590083691924783,0.591796779337622,0.593509866750461,
0.59375,0.595434222620651,0.597116189086285,0.598818775168995,0.600500384522268,
0.602213458969697,0.603926533417125,0.604166666666667,0.605850881513831,
0.607532821167997,0.609235415896949,0.610917025257753,0.612630112670779,
0.614343200083805,0.614583333333333,0.61626754818061,0.617949487835351,
0.619652082564126,0.621333691924504,0.623046779337477,0.62475986675045,
0.625,0.626684214847365,0.62836615450299,0.630068749231531,0.631750358591773,
0.633463446004463,0.635176533417153,0.635416666666667,0.637100881513971,
0.638782821168762,0.640485415897536,0.642167025258001,0.64388011267093,
0.645593200083859,0.645833333333333,0.647517548180316,0.649199487835431,
0.650902082564188,0.652583691924302,0.654296779337381,0.65600986675046,
0.65625,0.657934214847428,0.65961615450275,0.661318749231359,0.663000358591569,
0.664713446004377,0.666426533417185,0.666666666666667,0.668350881513661,
0.670032821169161,0.671735415897832,0.673417025258327,0.675130112671086,
0.676843200083846,0.677083333333333,0.678767548180001,0.680449487835573,
0.682152082564307,0.683833691924787,0.685546779337648,0.68725986675051,
0.6875,0.689184214847388,0.6908661545025,0.692568749231162,0.69425035859202,
0.695963446004585,0.69767653341715,0.697916666666667,0.699600881514463,
0.70128282116929,0.702985415897923,0.70466702525867,0.706380112671246,0.708093200083822,
0.708333333333333,0.710017548180411,0.711699487835929,0.713402082564578,
0.715083691925223,0.716796779337875,0.718509866750527,0.71875,0.720434214846616,
0.72211615450235,0.723818749231043,0.725500358591602,0.727213446004362,
0.728926533417123,0.729166666666667,0.730850881513419,0.732532821169214,
0.73423541589785,0.735917025258065,0.737630112670911,0.739343200083758,
0.739583333333333,0.741267548180221,0.742949487835294,0.744652082564087,
0.746333691924615,0.748046779337542,0.749759866750469,0.75,0.751684214846416,
0.753366154502443,0.755068749231134,0.756750358591587,0.758463446004397,
0.760176533417206,0.760416666666667,0.762100881513496,0.763782821168422,
0.765485415897281,0.767167025257607,0.768880112670732,0.770593200083858,
0.770833333333333,0.772517548179594,0.774199487835344,0.775902082564116,
0.777583691924374,0.779296779337404,0.781009866750434,0.78125,0.78293421484669,
0.784616154502112,0.786318749230868,0.788000358591228,0.789713446004183,
0.791426533417138,0.791666666666667,0.793350881513279,0.795032821168849,
0.796735415897573,0.798417025258128,0.800130112670938,0.801843200083748,
0.802083333333333,0.80376754817991,0.805449487834996,0.807152082563882,
0.808833691924143,0.810546779337342,0.81225986675054,0.8125,0.814184214846875,
0.815866154502397,0.817568749231082,0.819250358591479,0.820963446004308,
0.822676533417138,0.822916666666667,0.824600881513549,0.82628282116942,
0.827985415898024,0.829667025258528,0.831380112671183,0.833093200083837,
0.833333333333333,0.835017548180832,0.836699487835411,0.838402082564181,
0.840083691924666,0.841796779337578,0.843509866750491,0.84375,0.845434214847378,
0.847116154502397,0.84881874923109,0.850500358591155,0.852213446004163,
0.853926533417171,0.854166666666667,0.855850881513812,0.857532821168573,
0.859235415897376,0.860917025258013,0.862630112670899,0.864343200083785,
0.864583333333333,0.866267548179718,0.867949487835134,0.86965208256396,
0.871333691924431,0.873046779337435,0.874759866750439,0.875,0.876684214846492,
0.878366154501995,0.880068749230787,0.881750358591456,0.88346344600431,
0.885176533417163,0.885416666666667,0.887100881513135,0.888782821168991,
0.890485415897707,0.892167025258341,0.893880112671098,0.895593200083855,
0.895833333333333,0.897517548179665,0.899199487834624,0.900902082563594,
0.902583691923825,0.904296779337165,0.906009866750505,0.90625,0.907934214846278,
0.909616154501992,0.91131874923077,0.913000358591198,0.914713446004152,
0.916426533417106,0.916666666666667,0.918350881512217,0.920032821168928,
0.921735415897672,0.923417025258493,0.925130112671199,0.926843200083906,
0.927083333333333,0.928767548179258,0.93044948783491,0.932152082563814,
0.933833691923954,0.935546779337241,0.937259866750527,0.9375,0.939184214847346,
0.940866154502457,0.942568749231125,0.94425035859122,0.945963446004174,
0.947676533417128,0.947916666666667,0.949600881513474,0.951282821169022,
0.952985415897738,0.95466702525834,0.956380112671114,0.958093200083887,
0.958333333333333,0.960017548181036,0.961699487835379,0.963402082564164,
0.965083691924602,0.966796779337562,0.968509866750522,0.96875,0.970434214847239,
0.972116154502219,0.973818749230962,0.975500358591352,0.977213446004272,
0.978926533417192,0.979166666666667,0.980850881513793,0.982532821168591,
0.98423541589741,0.985917025258421,0.987630112671144,0.989343200083866,
0.989583333333333,0.991267548181292,0.992949487836093,0.994652082564706,
0.996333691925092,0.998046779337818,0.999759866750545,1.),.UNSPECIFIED.);
#127=B_SPLINE_CURVE_WITH_KNOTS('',3,(#11295,#11296,#11297,#11298,#11299,
#11300,#11301,#11302,#11303,#11304,#11305,#11306),.UNSPECIFIED.,.F.,.F.,
(4,2,2,2,2,4),(2.72017260531256E-6,0.00801802930125374,0.0194025153047282,
0.0282740905432685,0.0382285674272786,0.0405127362382465),.UNSPECIFIED.);
#128=B_SPLINE_CURVE_WITH_KNOTS('',3,(#11775,#11776,#11777,#11778,#11779,
#11780,#11781,#11782,#11783,#11784,#11785,#11786,#11787,#11788,#11789,#11790,
#11791,#11792,#11793,#11794,#11795,#11796,#11797,#11798,#11799,#11800,#11801,
#11802,#11803,#11804,#11805,#11806,#11807,#11808,#11809,#11810,#11811,#11812,
#11813,#11814,#11815,#11816,#11817,#11818),.UNSPECIFIED.,.F.,.F.,(4,1,1,
1,1,1,1,1,1,1,1,1,1,1,1,1,1,1,1,1,1,1,1,1,1,1,1,1,1,1,1,1,1,1,1,1,1,1,1,
1,1,4),(0.,0.0155086969164078,0.0371731810819821,0.0514015376726156,0.0721494932844473,
0.0879462852339701,0.102136934793609,0.118096046183078,0.19862023937012,
0.220465782155634,0.23365418085247,0.241548051822006,0.250379403180355,
0.265039089454663,0.283941482221575,0.302847655089067,0.314345531734621,
0.357463421988275,0.386547700128901,0.416631362178992,0.447827251721429,
0.480835486339271,0.507932786796811,0.529341861229807,0.553738573125003,
0.594012510221834,0.628912316880978,0.64568724667197,0.66015205447044,0.674349782601168,
0.687580075802142,0.700468884473892,0.724215901035998,0.747660515873313,
0.770169322257755,0.837047273198873,0.898018999477543,0.927421383188233,
0.952466294986228,0.96568815856341,0.980894474823001,1.),.UNSPECIFIED.);
#129=B_SPLINE_CURVE_WITH_KNOTS('',3,(#11822,#11823,#11824,#11825,#11826,
#11827,#11828,#11829,#11830,#11831,#11832,#11833,#11834,#11835,#11836,#11837,
#11838,#11839,#11840,#11841,#11842,#11843,#11844,#11845,#11846,#11847,#11848,
#11849,#11850,#11851,#11852,#11853,#11854,#11855,#11856,#11857,#11858,#11859,
#11860,#11861,#11862,#11863,#11864,#11865),.UNSPECIFIED.,.F.,.F.,(4,1,1,
1,1,1,1,1,1,1,1,1,1,1,1,1,1,1,1,1,1,1,1,1,1,1,1,1,1,1,1,1,1,1,1,1,1,1,1,
1,1,4),(0.,0.0155086969164078,0.0371731810819821,0.0514015376726156,0.0721494932844473,
0.0879462852339701,0.102136934793609,0.118096046183078,0.19862023937012,
0.220465782155634,0.23365418085247,0.241548051822006,0.250379403180355,
0.265039089454663,0.283941482221575,0.302847655089067,0.314345531734621,
0.357463421988275,0.386547700128901,0.416631362178992,0.447827251721429,
0.480835486339271,0.507932786796811,0.529341861229807,0.553738573125003,
0.594012510221834,0.628912316880978,0.64568724667197,0.66015205447044,0.674349782601168,
0.687580075802142,0.700468884473892,0.724215901035998,0.747660515873313,
0.770169322257755,0.837047273198873,0.898018999477543,0.927421383188233,
0.952466294986228,0.96568815856341,0.980894474823001,1.),.UNSPECIFIED.);
#130=B_SPLINE_CURVE_WITH_KNOTS('',3,(#11878,#11879,#11880,#11881),
 .UNSPECIFIED.,.F.,.F.,(4,4),(0.,1.),.UNSPECIFIED.);
#131=B_SPLINE_CURVE_WITH_KNOTS('',3,(#11884,#11885,#11886,#11887),
 .UNSPECIFIED.,.F.,.F.,(4,4),(0.,1.),.UNSPECIFIED.);
#132=B_SPLINE_CURVE_WITH_KNOTS('',3,(#11901,#11902,#11903,#11904,#11905,
#11906),.UNSPECIFIED.,.F.,.F.,(4,1,1,4),(0.,0.470503009353909,0.684670022609357,
1.),.UNSPECIFIED.);
#133=B_SPLINE_CURVE_WITH_KNOTS('',3,(#11909,#11910,#11911,#11912,#11913,
#11914),.UNSPECIFIED.,.F.,.F.,(4,1,1,4),(0.,0.470503009353909,0.684670022609357,
1.),.UNSPECIFIED.);
#134=B_SPLINE_CURVE_WITH_KNOTS('',3,(#11926,#11927,#11928,#11929,#11930),
 .UNSPECIFIED.,.F.,.F.,(4,1,4),(0.,0.519782906107891,1.),.UNSPECIFIED.);
#135=B_SPLINE_CURVE_WITH_KNOTS('',3,(#11933,#11934,#11935,#11936,#11937),
 .UNSPECIFIED.,.F.,.F.,(4,1,4),(0.,0.519782906107891,1.),.UNSPECIFIED.);
#136=B_SPLINE_CURVE_WITH_KNOTS('',3,(#11952,#11953,#11954,#11955,#11956,
#11957,#11958),.UNSPECIFIED.,.F.,.F.,(4,1,1,1,4),(0.,0.490961406160804,
0.688676820334042,0.846051539210629,1.),.UNSPECIFIED.);
#137=B_SPLINE_CURVE_WITH_KNOTS('',3,(#11959,#11960,#11961,#11962,#11963,
#11964,#11965),.UNSPECIFIED.,.F.,.F.,(4,1,1,1,4),(0.,0.490961406160804,
0.688676820334042,0.846051539210629,1.),.UNSPECIFIED.);
#138=B_SPLINE_SURFACE_WITH_KNOTS('',3,1,((#2727,#2728),(#2729,#2730),(#2731,
#2732),(#2733,#2734),(#2735,#2736),(#2737,#2738),(#2739,#2740),(#2741,#2742),
(#2743,#2744),(#2745,#2746),(#2747,#2748),(#2749,#2750)),.UNSPECIFIED.,
 .F.,.F.,.F.,(4,1,1,1,1,1,1,1,1,4),(2,2),(0.692277335272932,0.69714998216664,
0.713058394872634,0.723664003343296,0.736358399716042,0.759577826910316,
0.780092040409136,0.810242072545427,0.901462701662728,0.958125874426747),
(0.,0.216),.UNSPECIFIED.);
#139=B_SPLINE_SURFACE_WITH_KNOTS('',3,1,((#2781,#2782),(#2783,#2784),(#2785,
#2786),(#2787,#2788),(#2789,#2790),(#2791,#2792)),.UNSPECIFIED.,.F.,.F.,
 .F.,(4,1,1,4),(2,2),(0.,0.587279823509184,0.66516934088919,1.),(0.,0.216),
 .UNSPECIFIED.);
#140=B_SPLINE_SURFACE_WITH_KNOTS('',3,1,((#2808,#2809),(#2810,#2811),(#2812,
#2813),(#2814,#2815),(#2816,#2817),(#2818,#2819),(#2820,#2821)),
 .UNSPECIFIED.,.F.,.F.,.F.,(4,1,1,1,4),(2,2),(0.,0.0866729836098282,0.459841695939614,
0.649673299675604,0.845208563176808),(0.,0.216000000047327),
 .UNSPECIFIED.);
#141=B_SPLINE_SURFACE_WITH_KNOTS('',1,3,((#3306,#3307,#3308,#3309,#3310,
#3311,#3312,#3313,#3314,#3315,#3316,#3317,#3318,#3319,#3320,#3321,#3322,
#3323,#3324,#3325,#3326,#3327,#3328,#3329,#3330,#3331,#3332,#3333,#3334,
#3335,#3336,#3337,#3338,#3339,#3340,#3341,#3342,#3343,#3344,#3345,#3346,
#3347,#3348,#3349,#3350,#3351,#3352,#3353,#3354,#3355,#3356,#3357,#3358,
#3359,#3360,#3361,#3362,#3363,#3364,#3365,#3366,#3367,#3368,#3369,#3370,
#3371,#3372,#3373,#3374,#3375,#3376,#3377,#3378,#3379,#3380,#3381,#3382,
#3383,#3384,#3385,#3386,#3387,#3388,#3389,#3390,#3391,#3392,#3393,#3394,
#3395,#3396,#3397,#3398,#3399,#3400,#3401,#3402,#3403,#3404,#3405,#3406,
#3407,#3408,#3409,#3410,#3411,#3412,#3413,#3414,#3415,#3416,#3417,#3418,
#3419,#3420,#3421,#3422,#3423,#3424,#3425,#3426,#3427,#3428,#3429,#3430,
#3431,#3432,#3433,#3434,#3435,#3436,#3437,#3438,#3439,#3440,#3441,#3442,
#3443,#3444,#3445,#3446,#3447,#3448,#3449,#3450,#3451,#3452,#3453,#3454,
#3455,#3456,#3457,#3458,#3459,#3460,#3461),(#3462,#3463,#3464,#3465,#3466,
#3467,#3468,#3469,#3470,#3471,#3472,#3473,#3474,#3475,#3476,#3477,#3478,
#3479,#3480,#3481,#3482,#3483,#3484,#3485,#3486,#3487,#3488,#3489,#3490,
#3491,#3492,#3493,#3494,#3495,#3496,#3497,#3498,#3499,#3500,#3501,#3502,
#3503,#3504,#3505,#3506,#3507,#3508,#3509,#3510,#3511,#3512,#3513,#3514,
#3515,#3516,#3517,#3518,#3519,#3520,#3521,#3522,#3523,#3524,#3525,#3526,
#3527,#3528,#3529,#3530,#3531,#3532,#3533,#3534,#3535,#3536,#3537,#3538,
#3539,#3540,#3541,#3542,#3543,#3544,#3545,#3546,#3547,#3548,#3549,#3550,
#3551,#3552,#3553,#3554,#3555,#3556,#3557,#3558,#3559,#3560,#3561,#3562,
#3563,#3564,#3565,#3566,#3567,#3568,#3569,#3570,#3571,#3572,#3573,#3574,
#3575,#3576,#3577,#3578,#3579,#3580,#3581,#3582,#3583,#3584,#3585,#3586,
#3587,#3588,#3589,#3590,#3591,#3592,#3593,#3594,#3595,#3596,#3597,#3598,
#3599,#3600,#3601,#3602,#3603,#3604,#3605,#3606,#3607,#3608,#3609,#3610,
#3611,#3612,#3613,#3614,#3615,#3616,#3617)),.UNSPECIFIED.,.F.,.F.,.F.,(2,
2),(4,2,2,2,2,2,2,2,2,2,2,2,2,2,2,2,2,2,2,2,2,2,2,2,2,2,2,2,2,2,2,2,2,2,
2,2,2,2,2,2,2,2,2,2,2,2,2,2,2,2,2,2,2,2,2,2,2,2,2,2,2,2,2,2,2,2,2,2,2,2,
2,2,2,2,2,2,2,4),(-2.82979241385037E-6,1.00000282979242),(0.0211247699785431,
0.0224166474384851,0.023062586168456,0.023708524898427,0.0240314942634125,
0.024354463628398,0.0246774329933834,0.0247581753346298,0.024798546505253,
0.0248389176758762,0.0248591032611878,0.0248792888464994,0.0248994744318109,
0.0249196600171225,0.0249600311877457,0.0250004023583689,0.0250811446996153,
0.0251618870408617,0.0253233717233544,0.0256463410883399,0.0259693104533254,
0.0262922798183108,0.0275841572782528,0.0288760347381947,0.0301679121981366,
0.0314597896580785,0.0321057283880495,0.0327516671180205,0.0333976058479914,
0.0340435445779624,0.0353354220379043,0.0366272994978462,0.0392110544177301,
0.040502931877672,0.0417948093376139,0.0430866867975558,0.0443785642574978,
0.0469623191773816,0.0495460740972655,0.0521298290171493,0.0547135839370332,
0.057297338856917,0.0585892163168589,0.0598810937768009,0.0624648486966847,
0.0676323585364524,0.0727998683762201,0.0753836232961039,0.0779673782159878,
0.0792592556759297,0.0805511331358716,0.0831348880557555,0.0857186429756393,
0.0883023978955232,0.090886152815407,0.0934699077352909,0.0947617851952328,
0.0960536626551747,0.0966996013851457,0.0970225707501312,0.0973455401151166,
0.0976685094801021,0.0979914788450876,0.0986374175750586,0.0992833563050295,
0.0999292950350005,0.100575233764971,0.101221172494942,0.101544141859928,
0.101867111224913,0.102028595907406,0.102190080589899,0.102270822931145,
0.102351565272392,0.102513049954884,0.10283601931987,0.103158988684855,
0.103804927414826),.UNSPECIFIED.);
#142=B_SPLINE_SURFACE_WITH_KNOTS('',3,1,((#3625,#3626),(#3627,#3628),(#3629,
#3630),(#3631,#3632),(#3633,#3634),(#3635,#3636),(#3637,#3638),(#3639,#3640)),
 .UNSPECIFIED.,.F.,.F.,.F.,(4,1,1,1,1,4),(2,2),(0.,0.156258367612318,0.290685780689375,
0.48035435867502,0.63435677163295,0.643520450564764),(0.,0.0719999999999998),
 .UNSPECIFIED.);
#143=B_SPLINE_SURFACE_WITH_KNOTS('',3,1,((#3663,#3664),(#3665,#3666),(#3667,
#3668),(#3669,#3670),(#3671,#3672),(#3673,#3674),(#3675,#3676),(#3677,#3678),
(#3679,#3680),(#3681,#3682),(#3683,#3684),(#3685,#3686)),.UNSPECIFIED.,
 .F.,.F.,.F.,(4,1,1,1,1,1,1,1,1,4),(2,2),(0.69108883441235,0.69714998216664,
0.713058394872634,0.723664003343296,0.736358399716042,0.759577826910316,
0.780092040409136,0.810242072545427,0.901462701662728,0.958125874426747),
(0.,0.216),.UNSPECIFIED.);
#144=B_SPLINE_SURFACE_WITH_KNOTS('',3,1,((#3847,#3848),(#3849,#3850),(#3851,
#3852),(#3853,#3854),(#3855,#3856),(#3857,#3858)),.UNSPECIFIED.,.F.,.F.,
 .F.,(4,1,1,4),(2,2),(0.,0.587279823509184,0.66516934088919,1.),(0.,0.216),
 .UNSPECIFIED.);
#145=B_SPLINE_SURFACE_WITH_KNOTS('',3,1,((#3874,#3875),(#3876,#3877),(#3878,
#3879),(#3880,#3881),(#3882,#3883),(#3884,#3885),(#3886,#3887)),
 .UNSPECIFIED.,.F.,.F.,.F.,(4,1,1,1,4),(2,2),(0.,0.0866729836098282,0.459841695939614,
0.649673299675604,0.845208563176808),(0.,0.216),.UNSPECIFIED.);
#146=B_SPLINE_SURFACE_WITH_KNOTS('',1,3,((#4325,#4326,#4327,#4328,#4329,
#4330,#4331,#4332,#4333,#4334,#4335,#4336,#4337,#4338,#4339,#4340,#4341,
#4342,#4343,#4344,#4345,#4346,#4347,#4348,#4349,#4350,#4351,#4352,#4353,
#4354,#4355,#4356,#4357,#4358,#4359,#4360,#4361,#4362,#4363,#4364,#4365,
#4366,#4367,#4368,#4369,#4370,#4371,#4372,#4373,#4374,#4375,#4376,#4377,
#4378,#4379,#4380,#4381,#4382,#4383,#4384,#4385,#4386,#4387,#4388,#4389,
#4390,#4391,#4392,#4393,#4394,#4395,#4396,#4397,#4398,#4399,#4400,#4401,
#4402,#4403,#4404,#4405,#4406,#4407,#4408,#4409,#4410,#4411,#4412,#4413),
(#4414,#4415,#4416,#4417,#4418,#4419,#4420,#4421,#4422,#4423,#4424,#4425,
#4426,#4427,#4428,#4429,#4430,#4431,#4432,#4433,#4434,#4435,#4436,#4437,
#4438,#4439,#4440,#4441,#4442,#4443,#4444,#4445,#4446,#4447,#4448,#4449,
#4450,#4451,#4452,#4453,#4454,#4455,#4456,#4457,#4458,#4459,#4460,#4461,
#4462,#4463,#4464,#4465,#4466,#4467,#4468,#4469,#4470,#4471,#4472,#4473,
#4474,#4475,#4476,#4477,#4478,#4479,#4480,#4481,#4482,#4483,#4484,#4485,
#4486,#4487,#4488,#4489,#4490,#4491,#4492,#4493,#4494,#4495,#4496,#4497,
#4498,#4499,#4500,#4501,#4502),(#4503,#4504,#4505,#4506,#4507,#4508,#4509,
#4510,#4511,#4512,#4513,#4514,#4515,#4516,#4517,#4518,#4519,#4520,#4521,
#4522,#4523,#4524,#4525,#4526,#4527,#4528,#4529,#4530,#4531,#4532,#4533,
#4534,#4535,#4536,#4537,#4538,#4539,#4540,#4541,#4542,#4543,#4544,#4545,
#4546,#4547,#4548,#4549,#4550,#4551,#4552,#4553,#4554,#4555,#4556,#4557,
#4558,#4559,#4560,#4561,#4562,#4563,#4564,#4565,#4566,#4567,#4568,#4569,
#4570,#4571,#4572,#4573,#4574,#4575,#4576,#4577,#4578,#4579,#4580,#4581,
#4582,#4583,#4584,#4585,#4586,#4587,#4588,#4589,#4590,#4591)),
 .UNSPECIFIED.,.F.,.F.,.F.,(2,1,2),(4,2,2,2,2,2,2,2,2,2,2,2,2,2,2,2,2,2,
2,2,2,2,2,2,2,2,2,2,2,2,2,2,2,2,2,2,2,2,2,2,2,2,3,4),(-1.65164793228187E-5,
1.,1.01),(0.00983313761878334,0.0132402569819186,0.0140920368227025,0.0145179267430944,
0.0147308717032903,0.0147841079433393,0.0148373441833883,0.0149438166634863,
0.016647376345054,0.0183509360266216,0.0192027158674054,0.0200544957081893,
0.0234616150713246,0.0251651747528922,0.0268687344344599,0.0302758537975952,
0.0336829731607305,0.0353865328422982,0.0370900925238658,0.0439043312501364,
0.0473114506132717,0.0507185699764071,0.0541256893395424,0.0575328087026777,
0.0579586986230696,0.0583845885434615,0.0592363683842453,0.0600881482250292,
0.0603010931852251,0.0604075656653231,0.0605140381454211,0.060726983105617,
0.060939928065813,0.0613658179862049,0.0617917079065968,0.0622175978269887,
0.0624305427871847,0.0626434877473806,0.0628564327075766,0.0630693776677726,
0.0634952675881645,0.0639211575085564,0.0643470474289483,0.0653812909954315),
 .UNSPECIFIED.);
#147=B_SPLINE_SURFACE_WITH_KNOTS('',2,1,((#4600,#4601),(#4602,#4603),(#4604,
#4605)),.UNSPECIFIED.,.F.,.F.,.F.,(3,3),(2,2),(0.,1.),(0.,0.0287999999999918),
 .UNSPECIFIED.);
#148=B_SPLINE_SURFACE_WITH_KNOTS('',3,1,((#4671,#4672),(#4673,#4674),(#4675,
#4676),(#4677,#4678),(#4679,#4680),(#4681,#4682)),.UNSPECIFIED.,.F.,.F.,
 .F.,(4,1,1,4),(2,2),(0.,0.494943232770503,0.789351610361564,1.),(0.,0.17280000000419),
 .UNSPECIFIED.);
#149=B_SPLINE_SURFACE_WITH_KNOTS('',3,1,((#4710,#4711),(#4712,#4713),(#4714,
#4715),(#4716,#4717),(#4718,#4719),(#4720,#4721),(#4722,#4723),(#4724,#4725),
(#4726,#4727),(#4728,#4729),(#4730,#4731),(#4732,#4733)),.UNSPECIFIED.,
 .F.,.F.,.F.,(4,1,1,1,1,1,1,1,1,4),(2,2),(0.0654911701302355,0.0728325313021349,
0.151642943092782,0.236641834545795,0.351573197840935,0.540150564955284,
0.71598472862448,0.797600110822501,0.875509677594327,1.),(0.,0.1728),
 .UNSPECIFIED.);
#150=B_SPLINE_SURFACE_WITH_KNOTS('',2,1,((#4764,#4765),(#4766,#4767),(#4768,
#4769)),.UNSPECIFIED.,.F.,.F.,.F.,(3,3),(2,2),(0.,1.),(0.,0.1728),
 .UNSPECIFIED.);
#151=B_SPLINE_SURFACE_WITH_KNOTS('',1,3,((#4861,#4862,#4863,#4864,#4865,
#4866,#4867,#4868,#4869,#4870,#4871,#4872,#4873,#4874,#4875,#4876,#4877,
#4878,#4879,#4880,#4881,#4882,#4883,#4884,#4885,#4886,#4887,#4888,#4889,
#4890,#4891,#4892,#4893,#4894,#4895,#4896,#4897,#4898,#4899,#4900,#4901,
#4902,#4903,#4904,#4905,#4906,#4907,#4908,#4909,#4910,#4911,#4912,#4913,
#4914,#4915,#4916,#4917,#4918,#4919,#4920,#4921,#4922,#4923,#4924,#4925,
#4926,#4927,#4928,#4929,#4930,#4931,#4932,#4933,#4934,#4935,#4936,#4937,
#4938,#4939,#4940),(#4941,#4942,#4943,#4944,#4945,#4946,#4947,#4948,#4949,
#4950,#4951,#4952,#4953,#4954,#4955,#4956,#4957,#4958,#4959,#4960,#4961,
#4962,#4963,#4964,#4965,#4966,#4967,#4968,#4969,#4970,#4971,#4972,#4973,
#4974,#4975,#4976,#4977,#4978,#4979,#4980,#4981,#4982,#4983,#4984,#4985,
#4986,#4987,#4988,#4989,#4990,#4991,#4992,#4993,#4994,#4995,#4996,#4997,
#4998,#4999,#5000,#5001,#5002,#5003,#5004,#5005,#5006,#5007,#5008,#5009,
#5010,#5011,#5012,#5013,#5014,#5015,#5016,#5017,#5018,#5019,#5020)),
 .UNSPECIFIED.,.F.,.F.,.F.,(2,2),(4,2,2,2,2,2,2,2,2,2,2,2,2,2,2,2,2,2,2,
2,2,2,2,2,2,2,2,2,2,2,2,2,2,2,2,2,2,2,2,4),(0.,1.),(0.0438296453716767,
0.0445782836066419,0.0449526027241245,0.0453269218416071,0.0457012409590896,
0.0458884005178309,0.0459819802972016,0.0460755600765722,0.0462627196353135,
0.0464498791940548,0.0468241983115374,0.0475728365465026,0.0483214747814677,
0.049818751251398,0.0528133041912587,0.0558078571311194,0.0573051336010497,
0.05880241007098,0.0617969630108407,0.0647915159507014,0.067786068890562,
0.0737751747702833,0.0797642806500047,0.0827588335898653,0.0842561100597957,
0.085753386529726,0.0872506629996563,0.0879993012346215,0.0887479394695867,
0.0891222585870692,0.0893094181458105,0.0894965777045518,0.0895901574839225,
0.0896837372632931,0.0898708968220344,0.0900580563807757,0.090245215939517,
0.0906195350569996,0.0909938541744821,0.0917424924094473),.UNSPECIFIED.);
#152=B_SPLINE_SURFACE_WITH_KNOTS('',3,1,((#5034,#5035),(#5036,#5037),(#5038,
#5039),(#5040,#5041)),.UNSPECIFIED.,.F.,.F.,.F.,(4,4),(2,2),(0.,1.),(0.,
0.1728),.UNSPECIFIED.);
#153=B_SPLINE_SURFACE_WITH_KNOTS('',2,1,((#5064,#5065),(#5066,#5067),(#5068,
#5069)),.UNSPECIFIED.,.F.,.F.,.F.,(3,3),(2,2),(0.,1.),(0.,0.0288000000000019),
 .UNSPECIFIED.);
#154=B_SPLINE_SURFACE_WITH_KNOTS('',3,1,((#5099,#5100),(#5101,#5102),(#5103,
#5104),(#5105,#5106),(#5107,#5108),(#5109,#5110),(#5111,#5112),(#5113,#5114),
(#5115,#5116),(#5117,#5118),(#5119,#5120),(#5121,#5122),(#5123,#5124),(#5125,
#5126),(#5127,#5128)),.UNSPECIFIED.,.F.,.F.,.F.,(4,1,1,1,1,1,1,1,1,1,1,
1,4),(2,2),(0.,0.157038713621339,0.211241890914945,0.295200207692272,0.373845032775918,
0.419097916699999,0.461946250305228,0.500883855221145,0.554258304196424,
0.580360336370224,0.654376236660092,0.774520045331176,1.),(0.,0.1728),
 .UNSPECIFIED.);
#155=B_SPLINE_SURFACE_WITH_KNOTS('',1,3,((#5193,#5194,#5195,#5196,#5197,
#5198,#5199,#5200,#5201,#5202,#5203,#5204,#5205,#5206,#5207,#5208,#5209,
#5210,#5211,#5212,#5213,#5214,#5215,#5216,#5217,#5218,#5219,#5220,#5221,
#5222),(#5223,#5224,#5225,#5226,#5227,#5228,#5229,#5230,#5231,#5232,#5233,
#5234,#5235,#5236,#5237,#5238,#5239,#5240,#5241,#5242,#5243,#5244,#5245,
#5246,#5247,#5248,#5249,#5250,#5251,#5252)),.UNSPECIFIED.,.F.,.F.,.F.,(2,
2),(4,2,2,2,2,2,2,2,2,2,2,2,2,2,4),(-6.70767833503595E-6,1.),(0.0508986734324183,
0.0527402705950223,0.0545818677576262,0.058265062082834,0.0619482564080419,
0.0656314507332498,0.0729978393836655,0.0803642280340812,0.0877306166844969,
0.0950970053349126,0.0987801996601205,0.102463393985328,0.106146588310536,
0.10798818547314,0.109829782635744),.UNSPECIFIED.);
#156=B_SPLINE_SURFACE_WITH_KNOTS('',3,1,((#11685,#11686),(#11687,#11688),
(#11689,#11690),(#11691,#11692),(#11693,#11694),(#11695,#11696),(#11697,
#11698),(#11699,#11700),(#11701,#11702),(#11703,#11704),(#11705,#11706),
(#11707,#11708),(#11709,#11710),(#11711,#11712),(#11713,#11714),(#11715,
#11716),(#11717,#11718),(#11719,#11720),(#11721,#11722),(#11723,#11724),
(#11725,#11726),(#11727,#11728),(#11729,#11730),(#11731,#11732),(#11733,
#11734),(#11735,#11736),(#11737,#11738),(#11739,#11740),(#11741,#11742),
(#11743,#11744),(#11745,#11746),(#11747,#11748),(#11749,#11750),(#11751,
#11752),(#11753,#11754),(#11755,#11756),(#11757,#11758),(#11759,#11760),
(#11761,#11762),(#11763,#11764),(#11765,#11766),(#11767,#11768),(#11769,
#11770),(#11771,#11772)),.UNSPECIFIED.,.F.,.F.,.F.,(4,1,1,1,1,1,1,1,1,1,
1,1,1,1,1,1,1,1,1,1,1,1,1,1,1,1,1,1,1,1,1,1,1,1,1,1,1,1,1,1,1,4),(2,2),
(0.,0.0155086969164078,0.0371731810819821,0.0514015376726156,0.0721494932844473,
0.0879462852339701,0.102136934793609,0.118096046183078,0.19862023937012,
0.220465782155634,0.23365418085247,0.241548051822006,0.250379403180355,
0.265039089454663,0.283941482221575,0.302847655089067,0.314345531734621,
0.357463421988275,0.386547700128901,0.416631362178992,0.447827251721429,
0.480835486339271,0.507932786796811,0.529341861229807,0.553738573125003,
0.594012510221834,0.628912316880978,0.64568724667197,0.66015205447044,0.674349782601168,
0.687580075802142,0.700468884473892,0.724215901035998,0.747660515873313,
0.770169322257755,0.837047273198873,0.898018999477543,0.927421383188233,
0.952466294986228,0.96568815856341,0.980894474823001,1.),(0.,0.1728),
 .UNSPECIFIED.);
#157=B_SPLINE_SURFACE_WITH_KNOTS('',3,1,((#11867,#11868),(#11869,#11870),
(#11871,#11872),(#11873,#11874),(#11875,#11876)),.UNSPECIFIED.,.F.,.F.,
 .F.,(4,1,4),(2,2),(0.,0.376046516805316,1.),(0.,0.1728),.UNSPECIFIED.);
#158=B_SPLINE_SURFACE_WITH_KNOTS('',3,1,((#11888,#11889),(#11890,#11891),
(#11892,#11893),(#11894,#11895),(#11896,#11897),(#11898,#11899)),
 .UNSPECIFIED.,.F.,.F.,.F.,(4,1,1,4),(2,2),(0.,0.470503009353909,0.684670022609357,
1.),(0.,0.1728),.UNSPECIFIED.);
#159=B_SPLINE_SURFACE_WITH_KNOTS('',3,1,((#11915,#11916),(#11917,#11918),
(#11919,#11920),(#11921,#11922),(#11923,#11924)),.UNSPECIFIED.,.F.,.F.,
 .F.,(4,1,4),(2,2),(0.,0.519782906107891,1.),(0.,0.1728),.UNSPECIFIED.);
#160=B_SPLINE_SURFACE_WITH_KNOTS('',3,1,((#11938,#11939),(#11940,#11941),
(#11942,#11943),(#11944,#11945),(#11946,#11947),(#11948,#11949),(#11950,
#11951)),.UNSPECIFIED.,.F.,.F.,.F.,(4,1,1,1,4),(2,2),(0.,0.490961406160804,
0.688676820334042,0.846051539210629,1.),(0.,0.1728),.UNSPECIFIED.);
#161=SHAPE_REPRESENTATION_RELATIONSHIP('SRR','None',#12184,#172);
#162=SHAPE_REPRESENTATION_RELATIONSHIP('SRR','None',#12185,#173);
#163=SHAPE_REPRESENTATION_RELATIONSHIP('SRR','None',#12186,#174);
#164=SHAPE_REPRESENTATION_RELATIONSHIP('SRR','None',#12188,#175);
#165=SHAPE_REPRESENTATION_RELATIONSHIP('SRR','None',#12189,#176);
#166=SHAPE_REPRESENTATION_RELATIONSHIP('SRR','None',#12190,#177);
#167=SHAPE_REPRESENTATION_RELATIONSHIP('SRR','None',#12191,#178);
#168=SHAPE_REPRESENTATION_RELATIONSHIP('SRR','None',#12192,#179);
#169=SHAPE_REPRESENTATION_RELATIONSHIP('SRR','None',#12193,#180);
#170=SHAPE_REPRESENTATION_RELATIONSHIP('SRR','None',#12194,#181);
#171=SHAPE_REPRESENTATION_RELATIONSHIP('SRR','None',#12195,#182);
#172=ADVANCED_BREP_SHAPE_REPRESENTATION('',(#194),#12125);
#173=ADVANCED_BREP_SHAPE_REPRESENTATION('',(#195),#12126);
#174=ADVANCED_BREP_SHAPE_REPRESENTATION('',(#196),#12127);
#175=ADVANCED_BREP_SHAPE_REPRESENTATION('',(#197),#12129);
#176=ADVANCED_BREP_SHAPE_REPRESENTATION('',(#198),#12130);
#177=ADVANCED_BREP_SHAPE_REPRESENTATION('',(#199),#12131);
#178=ADVANCED_BREP_SHAPE_REPRESENTATION('',(#200),#12132);
#179=ADVANCED_BREP_SHAPE_REPRESENTATION('',(#201),#12133);
#180=ADVANCED_BREP_SHAPE_REPRESENTATION('',(#202),#12134);
#181=ADVANCED_BREP_SHAPE_REPRESENTATION('',(#203),#12135);
#182=ADVANCED_BREP_SHAPE_REPRESENTATION('',(#204),#12136);
#183=STYLED_ITEM('',(#12253),#194);
#184=STYLED_ITEM('',(#12253),#195);
#185=STYLED_ITEM('',(#12253),#196);
#186=STYLED_ITEM('',(#12253),#197);
#187=STYLED_ITEM('',(#12253),#198);
#188=STYLED_ITEM('',(#12253),#199);
#189=STYLED_ITEM('',(#12253),#200);
#190=STYLED_ITEM('',(#12253),#201);
#191=STYLED_ITEM('',(#12253),#202);
#192=STYLED_ITEM('',(#12253),#203);
#193=STYLED_ITEM('',(#12253),#204);
#194=MANIFOLD_SOLID_BREP('Body1',#1828);
#195=MANIFOLD_SOLID_BREP('Body1',#1829);
#196=MANIFOLD_SOLID_BREP('Body1',#1830);
#197=MANIFOLD_SOLID_BREP('Body1',#1831);
#198=MANIFOLD_SOLID_BREP('Body1',#1832);
#199=MANIFOLD_SOLID_BREP('Body1',#1833);
#200=MANIFOLD_SOLID_BREP('Body1',#1834);
#201=MANIFOLD_SOLID_BREP('Body1',#1835);
#202=MANIFOLD_SOLID_BREP('Body1',#1836);
#203=MANIFOLD_SOLID_BREP('Body1',#1837);
#204=MANIFOLD_SOLID_BREP('Body1',#1838);
#205=FACE_BOUND('',#605,.T.);
#206=FACE_BOUND('',#606,.T.);
#207=FACE_BOUND('',#608,.T.);
#208=FACE_BOUND('',#609,.T.);
#209=FACE_BOUND('',#623,.T.);
#210=FACE_BOUND('',#625,.T.);
#211=FACE_BOUND('',#635,.T.);
#212=FACE_BOUND('',#637,.T.);
#213=FACE_BOUND('',#648,.T.);
#214=FACE_BOUND('',#650,.T.);
#215=FACE_BOUND('',#660,.T.);
#216=FACE_BOUND('',#661,.T.);
#217=FACE_BOUND('',#663,.T.);
#218=FACE_BOUND('',#664,.T.);
#219=FACE_BOUND('',#672,.T.);
#220=FACE_BOUND('',#680,.T.);
#221=FACE_BOUND('',#696,.T.);
#222=FACE_BOUND('',#698,.T.);
#223=FACE_BOUND('',#704,.T.);
#224=FACE_BOUND('',#705,.T.);
#225=FACE_BOUND('',#707,.T.);
#226=FACE_BOUND('',#708,.T.);
#227=FACE_BOUND('',#723,.T.);
#228=FACE_BOUND('',#728,.T.);
#229=FACE_BOUND('',#729,.T.);
#230=FACE_BOUND('',#731,.T.);
#231=FACE_BOUND('',#732,.T.);
#232=PLANE('',#1977);
#233=PLANE('',#1980);
#234=PLANE('',#1985);
#235=PLANE('',#1988);
#236=PLANE('',#2001);
#237=PLANE('',#2002);
#238=PLANE('',#2003);
#239=PLANE('',#2004);
#240=PLANE('',#2009);
#241=PLANE('',#2010);
#242=PLANE('',#2011);
#243=PLANE('',#2012);
#244=PLANE('',#2018);
#245=PLANE('',#2019);
#246=PLANE('',#2020);
#247=PLANE('',#2021);
#248=PLANE('',#2030);
#249=PLANE('',#2031);
#250=PLANE('',#2032);
#251=PLANE('',#2033);
#252=PLANE('',#2034);
#253=PLANE('',#2035);
#254=PLANE('',#2043);
#255=PLANE('',#2044);
#256=PLANE('',#2045);
#257=PLANE('',#2062);
#258=PLANE('',#2065);
#259=PLANE('',#2069);
#260=PLANE('',#2070);
#261=PLANE('',#2071);
#262=PLANE('',#2073);
#263=PLANE('',#2078);
#264=PLANE('',#2079);
#265=PLANE('',#2095);
#266=PLANE('',#2098);
#267=PLANE('',#2103);
#268=PLANE('',#2106);
#269=PLANE('',#2128);
#270=PLANE('',#2129);
#271=PLANE('',#2130);
#272=PLANE('',#2138);
#273=PLANE('',#2141);
#274=PLANE('',#2145);
#275=PLANE('',#2147);
#276=LINE('',#2672,#370);
#277=LINE('',#2676,#371);
#278=LINE('',#2683,#372);
#279=LINE('',#2686,#373);
#280=LINE('',#2692,#374);
#281=LINE('',#2695,#375);
#282=LINE('',#2698,#376);
#283=LINE('',#2701,#377);
#284=LINE('',#2704,#378);
#285=LINE('',#2705,#379);
#286=LINE('',#2708,#380);
#287=LINE('',#2711,#381);
#288=LINE('',#2725,#382);
#289=LINE('',#2766,#383);
#290=LINE('',#2780,#384);
#291=LINE('',#2801,#385);
#292=LINE('',#3179,#386);
#293=LINE('',#3180,#387);
#294=LINE('',#3183,#388);
#295=LINE('',#3185,#389);
#296=LINE('',#3304,#390);
#297=LINE('',#3623,#391);
#298=LINE('',#3643,#392);
#299=LINE('',#3654,#393);
#300=LINE('',#3832,#394);
#301=LINE('',#3846,#395);
#302=LINE('',#3867,#396);
#303=LINE('',#4298,#397);
#304=LINE('',#4299,#398);
#305=LINE('',#4302,#399);
#306=LINE('',#4303,#400);
#307=LINE('',#4598,#401);
#308=LINE('',#4608,#402);
#309=LINE('',#4667,#403);
#310=LINE('',#4704,#404);
#311=LINE('',#4736,#405);
#312=LINE('',#4751,#406);
#313=LINE('',#4775,#407);
#314=LINE('',#4781,#408);
#315=LINE('',#4788,#409);
#316=LINE('',#4790,#410);
#317=LINE('',#4859,#411);
#318=LINE('',#5026,#412);
#319=LINE('',#5032,#413);
#320=LINE('',#5057,#414);
#321=LINE('',#5063,#415);
#322=LINE('',#5097,#416);
#323=LINE('',#5147,#417);
#324=LINE('',#5164,#418);
#325=LINE('',#5166,#419);
#326=LINE('',#5167,#420);
#327=LINE('',#5170,#421);
#328=LINE('',#5172,#422);
#329=LINE('',#5173,#423);
#330=LINE('',#5177,#424);
#331=LINE('',#5185,#425);
#332=LINE('',#5186,#426);
#333=LINE('',#5188,#427);
#334=LINE('',#5189,#428);
#335=LINE('',#5191,#429);
#336=LINE('',#5258,#430);
#337=LINE('',#5264,#431);
#338=LINE('',#9938,#432);
#339=LINE('',#9942,#433);
#340=LINE('',#11683,#434);
#341=LINE('',#11820,#435);
#342=LINE('',#11866,#436);
#343=LINE('',#11883,#437);
#344=LINE('',#11908,#438);
#345=LINE('',#11932,#439);
#346=LINE('',#11987,#440);
#347=LINE('',#11991,#441);
#348=LINE('',#11998,#442);
#349=LINE('',#12001,#443);
#350=LINE('',#12007,#444);
#351=LINE('',#12010,#445);
#352=LINE('',#12013,#446);
#353=LINE('',#12016,#447);
#354=LINE('',#12019,#448);
#355=LINE('',#12020,#449);
#356=LINE('',#12023,#450);
#357=LINE('',#12026,#451);
#358=LINE('',#12052,#452);
#359=LINE('',#12055,#453);
#360=LINE('',#12064,#454);
#361=LINE('',#12070,#455);
#362=LINE('',#12077,#456);
#363=LINE('',#12080,#457);
#364=LINE('',#12086,#458);
#365=LINE('',#12089,#459);
#366=LINE('',#12091,#460);
#367=LINE('',#12092,#461);
#368=LINE('',#12094,#462);
#369=LINE('',#12096,#463);
#370=VECTOR('',#2186,2.);
#371=VECTOR('',#2191,2.);
#372=VECTOR('',#2198,1000.);
#373=VECTOR('',#2201,1000.);
#374=VECTOR('',#2206,1000.);
#375=VECTOR('',#2209,1000.);
#376=VECTOR('',#2212,1000.);
#377=VECTOR('',#2215,1000.);
#378=VECTOR('',#2218,1000.);
#379=VECTOR('',#2219,1000.);
#380=VECTOR('',#2222,1000.);
#381=VECTOR('',#2227,1000.);
#382=VECTOR('',#2250,2.);
#383=VECTOR('',#2253,1000.);
#384=VECTOR('',#2254,1000.);
#385=VECTOR('',#2255,1000.);
#386=VECTOR('',#2258,1000.);
#387=VECTOR('',#2259,1000.);
#388=VECTOR('',#2262,1000.);
#389=VECTOR('',#2263,1000.);
#390=VECTOR('',#2266,1000.);
#391=VECTOR('',#2275,2.00000000000001);
#392=VECTOR('',#2278,1000.);
#393=VECTOR('',#2279,1000.);
#394=VECTOR('',#2280,1000.);
#395=VECTOR('',#2281,1000.);
#396=VECTOR('',#2282,1000.);
#397=VECTOR('',#2287,1000.);
#398=VECTOR('',#2288,1000.);
#399=VECTOR('',#2291,1000.);
#400=VECTOR('',#2292,10.);
#401=VECTOR('',#2303,1.);
#402=VECTOR('',#2306,1000.);
#403=VECTOR('',#2307,1000.);
#404=VECTOR('',#2308,1000.);
#405=VECTOR('',#2309,1000.);
#406=VECTOR('',#2310,1000.);
#407=VECTOR('',#2311,1000.);
#408=VECTOR('',#2314,10.);
#409=VECTOR('',#2315,10.);
#410=VECTOR('',#2318,1000.);
#411=VECTOR('',#2321,1000.);
#412=VECTOR('',#2330,2.00000000000001);
#413=VECTOR('',#2337,1.);
#414=VECTOR('',#2340,1000.);
#415=VECTOR('',#2341,1000.);
#416=VECTOR('',#2342,1000.);
#417=VECTOR('',#2345,1000.);
#418=VECTOR('',#2346,1000.);
#419=VECTOR('',#2349,10.);
#420=VECTOR('',#2350,10.);
#421=VECTOR('',#2353,1000.);
#422=VECTOR('',#2354,1000.);
#423=VECTOR('',#2355,1000.);
#424=VECTOR('',#2358,1000.);
#425=VECTOR('',#2359,1000.);
#426=VECTOR('',#2360,1000.);
#427=VECTOR('',#2363,10.);
#428=VECTOR('',#2364,1000.);
#429=VECTOR('',#2367,1000.);
#430=VECTOR('',#2376,1.);
#431=VECTOR('',#2383,1.5);
#432=VECTOR('',#2428,1000.);
#433=VECTOR('',#2433,1000.);
#434=VECTOR('',#2456,2.00000000000001);
#435=VECTOR('',#2459,1000.);
#436=VECTOR('',#2460,1000.);
#437=VECTOR('',#2461,1000.);
#438=VECTOR('',#2462,1000.);
#439=VECTOR('',#2463,1000.);
#440=VECTOR('',#2492,2.);
#441=VECTOR('',#2497,2.);
#442=VECTOR('',#2504,1000.);
#443=VECTOR('',#2507,1000.);
#444=VECTOR('',#2512,1000.);
#445=VECTOR('',#2515,1000.);
#446=VECTOR('',#2518,1000.);
#447=VECTOR('',#2521,1000.);
#448=VECTOR('',#2524,1000.);
#449=VECTOR('',#2525,1000.);
#450=VECTOR('',#2528,1000.);
#451=VECTOR('',#2533,1000.);
#452=VECTOR('',#2572,2.);
#453=VECTOR('',#2577,4.);
#454=VECTOR('',#2590,2.);
#455=VECTOR('',#2597,2.00000000000001);
#456=VECTOR('',#2604,1000.);
#457=VECTOR('',#2607,1000.);
#458=VECTOR('',#2612,1000.);
#459=VECTOR('',#2615,1000.);
#460=VECTOR('',#2618,1000.);
#461=VECTOR('',#2619,1000.);
#462=VECTOR('',#2622,1000.);
#463=VECTOR('',#2625,1000.);
#464=CYLINDRICAL_SURFACE('',#1973,2.);
#465=CYLINDRICAL_SURFACE('',#1975,2.);
#466=CYLINDRICAL_SURFACE('',#1983,12.2723008899906);
#467=CYLINDRICAL_SURFACE('',#1986,12.2723008899906);
#468=CYLINDRICAL_SURFACE('',#1989,0.5);
#469=CYLINDRICAL_SURFACE('',#1996,0.5);
#470=CYLINDRICAL_SURFACE('',#1998,2.);
#471=CYLINDRICAL_SURFACE('',#2006,2.00000000000001);
#472=CYLINDRICAL_SURFACE('',#2015,1.);
#473=CYLINDRICAL_SURFACE('',#2023,2.00000000000001);
#474=CYLINDRICAL_SURFACE('',#2026,1.);
#475=CYLINDRICAL_SURFACE('',#2037,1.);
#476=CYLINDRICAL_SURFACE('',#2040,1.5);
#477=CYLINDRICAL_SURFACE('',#2075,2.00000000000001);
#478=CYLINDRICAL_SURFACE('',#2091,2.);
#479=CYLINDRICAL_SURFACE('',#2093,2.);
#480=CYLINDRICAL_SURFACE('',#2101,12.2723008899906);
#481=CYLINDRICAL_SURFACE('',#2104,12.2723008899906);
#482=CYLINDRICAL_SURFACE('',#2107,0.5);
#483=CYLINDRICAL_SURFACE('',#2114,0.5);
#484=CYLINDRICAL_SURFACE('',#2124,2.);
#485=CYLINDRICAL_SURFACE('',#2127,4.);
#486=CYLINDRICAL_SURFACE('',#2132,2.);
#487=CYLINDRICAL_SURFACE('',#2135,2.00000000000001);
#488=CYLINDRICAL_SURFACE('',#2144,9.00000000000003);
#489=CYLINDRICAL_SURFACE('',#2146,9.00000000000005);
#490=FACE_OUTER_BOUND('',#600,.T.);
#491=FACE_OUTER_BOUND('',#601,.T.);
#492=FACE_OUTER_BOUND('',#602,.T.);
#493=FACE_OUTER_BOUND('',#603,.T.);
#494=FACE_OUTER_BOUND('',#604,.T.);
#495=FACE_OUTER_BOUND('',#607,.T.);
#496=FACE_OUTER_BOUND('',#610,.T.);
#497=FACE_OUTER_BOUND('',#611,.T.);
#498=FACE_OUTER_BOUND('',#612,.T.);
#499=FACE_OUTER_BOUND('',#613,.T.);
#500=FACE_OUTER_BOUND('',#614,.T.);
#501=FACE_OUTER_BOUND('',#615,.T.);
#502=FACE_OUTER_BOUND('',#616,.T.);
#503=FACE_OUTER_BOUND('',#617,.T.);
#504=FACE_OUTER_BOUND('',#618,.T.);
#505=FACE_OUTER_BOUND('',#619,.T.);
#506=FACE_OUTER_BOUND('',#620,.T.);
#507=FACE_OUTER_BOUND('',#621,.T.);
#508=FACE_OUTER_BOUND('',#622,.T.);
#509=FACE_OUTER_BOUND('',#624,.T.);
#510=FACE_OUTER_BOUND('',#626,.T.);
#511=FACE_OUTER_BOUND('',#627,.T.);
#512=FACE_OUTER_BOUND('',#628,.T.);
#513=FACE_OUTER_BOUND('',#629,.T.);
#514=FACE_OUTER_BOUND('',#630,.T.);
#515=FACE_OUTER_BOUND('',#631,.T.);
#516=FACE_OUTER_BOUND('',#632,.T.);
#517=FACE_OUTER_BOUND('',#633,.T.);
#518=FACE_OUTER_BOUND('',#634,.T.);
#519=FACE_OUTER_BOUND('',#636,.T.);
#520=FACE_OUTER_BOUND('',#638,.T.);
#521=FACE_OUTER_BOUND('',#639,.T.);
#522=FACE_OUTER_BOUND('',#640,.T.);
#523=FACE_OUTER_BOUND('',#641,.T.);
#524=FACE_OUTER_BOUND('',#642,.T.);
#525=FACE_OUTER_BOUND('',#643,.T.);
#526=FACE_OUTER_BOUND('',#644,.T.);
#527=FACE_OUTER_BOUND('',#645,.T.);
#528=FACE_OUTER_BOUND('',#646,.T.);
#529=FACE_OUTER_BOUND('',#647,.T.);
#530=FACE_OUTER_BOUND('',#649,.T.);
#531=FACE_OUTER_BOUND('',#651,.T.);
#532=FACE_OUTER_BOUND('',#652,.T.);
#533=FACE_OUTER_BOUND('',#653,.T.);
#534=FACE_OUTER_BOUND('',#654,.T.);
#535=FACE_OUTER_BOUND('',#655,.T.);
#536=FACE_OUTER_BOUND('',#656,.T.);
#537=FACE_OUTER_BOUND('',#657,.T.);
#538=FACE_OUTER_BOUND('',#658,.T.);
#539=FACE_OUTER_BOUND('',#659,.T.);
#540=FACE_OUTER_BOUND('',#662,.T.);
#541=FACE_OUTER_BOUND('',#665,.T.);
#542=FACE_OUTER_BOUND('',#666,.T.);
#543=FACE_OUTER_BOUND('',#667,.T.);
#544=FACE_OUTER_BOUND('',#668,.T.);
#545=FACE_OUTER_BOUND('',#669,.T.);
#546=FACE_OUTER_BOUND('',#670,.T.);
#547=FACE_OUTER_BOUND('',#671,.T.);
#548=FACE_OUTER_BOUND('',#673,.T.);
#549=FACE_OUTER_BOUND('',#674,.T.);
#550=FACE_OUTER_BOUND('',#675,.T.);
#551=FACE_OUTER_BOUND('',#676,.T.);
#552=FACE_OUTER_BOUND('',#677,.T.);
#553=FACE_OUTER_BOUND('',#678,.T.);
#554=FACE_OUTER_BOUND('',#679,.T.);
#555=FACE_OUTER_BOUND('',#681,.T.);
#556=FACE_OUTER_BOUND('',#682,.T.);
#557=FACE_OUTER_BOUND('',#683,.T.);
#558=FACE_OUTER_BOUND('',#684,.T.);
#559=FACE_OUTER_BOUND('',#685,.T.);
#560=FACE_OUTER_BOUND('',#686,.T.);
#561=FACE_OUTER_BOUND('',#687,.T.);
#562=FACE_OUTER_BOUND('',#688,.T.);
#563=FACE_OUTER_BOUND('',#689,.T.);
#564=FACE_OUTER_BOUND('',#690,.T.);
#565=FACE_OUTER_BOUND('',#691,.T.);
#566=FACE_OUTER_BOUND('',#692,.T.);
#567=FACE_OUTER_BOUND('',#693,.T.);
#568=FACE_OUTER_BOUND('',#694,.T.);
#569=FACE_OUTER_BOUND('',#695,.T.);
#570=FACE_OUTER_BOUND('',#697,.T.);
#571=FACE_OUTER_BOUND('',#699,.T.);
#572=FACE_OUTER_BOUND('',#700,.T.);
#573=FACE_OUTER_BOUND('',#701,.T.);
#574=FACE_OUTER_BOUND('',#702,.T.);
#575=FACE_OUTER_BOUND('',#703,.T.);
#576=FACE_OUTER_BOUND('',#706,.T.);
#577=FACE_OUTER_BOUND('',#709,.T.);
#578=FACE_OUTER_BOUND('',#710,.T.);
#579=FACE_OUTER_BOUND('',#711,.T.);
#580=FACE_OUTER_BOUND('',#712,.T.);
#581=FACE_OUTER_BOUND('',#713,.T.);
#582=FACE_OUTER_BOUND('',#714,.T.);
#583=FACE_OUTER_BOUND('',#715,.T.);
#584=FACE_OUTER_BOUND('',#716,.T.);
#585=FACE_OUTER_BOUND('',#717,.T.);
#586=FACE_OUTER_BOUND('',#718,.T.);
#587=FACE_OUTER_BOUND('',#719,.T.);
#588=FACE_OUTER_BOUND('',#720,.T.);
#589=FACE_OUTER_BOUND('',#721,.T.);
#590=FACE_OUTER_BOUND('',#722,.T.);
#591=FACE_OUTER_BOUND('',#724,.T.);
#592=FACE_OUTER_BOUND('',#725,.T.);
#593=FACE_OUTER_BOUND('',#726,.T.);
#594=FACE_OUTER_BOUND('',#727,.T.);
#595=FACE_OUTER_BOUND('',#730,.T.);
#596=FACE_OUTER_BOUND('',#733,.T.);
#597=FACE_OUTER_BOUND('',#734,.T.);
#598=FACE_OUTER_BOUND('',#735,.T.);
#599=FACE_OUTER_BOUND('',#736,.T.);
#600=EDGE_LOOP('',(#1223,#1224,#1225,#1226,#1227));
#601=EDGE_LOOP('',(#1228,#1229,#1230,#1231,#1232));
#602=EDGE_LOOP('',(#1233,#1234,#1235,#1236,#1237));
#603=EDGE_LOOP('',(#1238,#1239,#1240,#1241,#1242));
#604=EDGE_LOOP('',(#1243,#1244,#1245,#1246));
#605=EDGE_LOOP('',(#1247));
#606=EDGE_LOOP('',(#1248));
#607=EDGE_LOOP('',(#1249,#1250,#1251,#1252));
#608=EDGE_LOOP('',(#1253));
#609=EDGE_LOOP('',(#1254));
#610=EDGE_LOOP('',(#1255,#1256,#1257,#1258));
#611=EDGE_LOOP('',(#1259,#1260,#1261,#1262));
#612=EDGE_LOOP('',(#1263,#1264,#1265,#1266));
#613=EDGE_LOOP('',(#1267,#1268,#1269,#1270));
#614=EDGE_LOOP('',(#1271,#1272,#1273,#1274));
#615=EDGE_LOOP('',(#1275,#1276,#1277,#1278));
#616=EDGE_LOOP('',(#1279,#1280,#1281,#1282));
#617=EDGE_LOOP('',(#1283,#1284,#1285,#1286));
#618=EDGE_LOOP('',(#1287,#1288,#1289,#1290));
#619=EDGE_LOOP('',(#1291,#1292,#1293,#1294));
#620=EDGE_LOOP('',(#1295,#1296,#1297,#1298));
#621=EDGE_LOOP('',(#1299,#1300,#1301,#1302));
#622=EDGE_LOOP('',(#1303,#1304,#1305,#1306,#1307,#1308));
#623=EDGE_LOOP('',(#1309));
#624=EDGE_LOOP('',(#1310,#1311,#1312,#1313,#1314,#1315));
#625=EDGE_LOOP('',(#1316));
#626=EDGE_LOOP('',(#1317,#1318,#1319,#1320));
#627=EDGE_LOOP('',(#1321,#1322,#1323,#1324));
#628=EDGE_LOOP('',(#1325,#1326,#1327,#1328));
#629=EDGE_LOOP('',(#1329,#1330,#1331,#1332));
#630=EDGE_LOOP('',(#1333,#1334,#1335,#1336));
#631=EDGE_LOOP('',(#1337,#1338,#1339,#1340,#1341));
#632=EDGE_LOOP('',(#1342,#1343,#1344,#1345));
#633=EDGE_LOOP('',(#1346,#1347,#1348,#1349,#1350));
#634=EDGE_LOOP('',(#1351,#1352,#1353,#1354));
#635=EDGE_LOOP('',(#1355));
#636=EDGE_LOOP('',(#1356,#1357,#1358,#1359,#1360,#1361));
#637=EDGE_LOOP('',(#1362));
#638=EDGE_LOOP('',(#1363,#1364,#1365,#1366));
#639=EDGE_LOOP('',(#1367,#1368,#1369,#1370));
#640=EDGE_LOOP('',(#1371,#1372,#1373,#1374,#1375,#1376));
#641=EDGE_LOOP('',(#1377,#1378,#1379,#1380));
#642=EDGE_LOOP('',(#1381,#1382,#1383,#1384));
#643=EDGE_LOOP('',(#1385,#1386,#1387,#1388,#1389));
#644=EDGE_LOOP('',(#1390,#1391,#1392,#1393));
#645=EDGE_LOOP('',(#1394,#1395,#1396,#1397));
#646=EDGE_LOOP('',(#1398,#1399,#1400,#1401,#1402));
#647=EDGE_LOOP('',(#1403,#1404,#1405,#1406,#1407,#1408));
#648=EDGE_LOOP('',(#1409));
#649=EDGE_LOOP('',(#1410,#1411,#1412,#1413,#1414,#1415));
#650=EDGE_LOOP('',(#1416));
#651=EDGE_LOOP('',(#1417,#1418,#1419,#1420));
#652=EDGE_LOOP('',(#1421,#1422,#1423,#1424));
#653=EDGE_LOOP('',(#1425,#1426,#1427,#1428));
#654=EDGE_LOOP('',(#1429,#1430,#1431,#1432));
#655=EDGE_LOOP('',(#1433,#1434,#1435,#1436,#1437));
#656=EDGE_LOOP('',(#1438,#1439,#1440,#1441));
#657=EDGE_LOOP('',(#1442,#1443,#1444,#1445));
#658=EDGE_LOOP('',(#1446,#1447,#1448,#1449));
#659=EDGE_LOOP('',(#1450,#1451,#1452,#1453,#1454,#1455,#1456));
#660=EDGE_LOOP('',(#1457));
#661=EDGE_LOOP('',(#1458));
#662=EDGE_LOOP('',(#1459,#1460,#1461,#1462,#1463,#1464,#1465));
#663=EDGE_LOOP('',(#1466));
#664=EDGE_LOOP('',(#1467));
#665=EDGE_LOOP('',(#1468,#1469,#1470,#1471,#1472));
#666=EDGE_LOOP('',(#1473,#1474,#1475,#1476));
#667=EDGE_LOOP('',(#1477,#1478,#1479,#1480));
#668=EDGE_LOOP('',(#1481,#1482,#1483,#1484));
#669=EDGE_LOOP('',(#1485,#1486,#1487,#1488));
#670=EDGE_LOOP('',(#1489,#1490,#1491,#1492));
#671=EDGE_LOOP('',(#1493));
#672=EDGE_LOOP('',(#1494));
#673=EDGE_LOOP('',(#1495));
#674=EDGE_LOOP('',(#1496));
#675=EDGE_LOOP('',(#1497,#1498,#1499,#1500,#1501));
#676=EDGE_LOOP('',(#1502,#1503,#1504,#1505,#1506));
#677=EDGE_LOOP('',(#1507,#1508,#1509,#1510,#1511));
#678=EDGE_LOOP('',(#1512,#1513,#1514,#1515,#1516,#1517));
#679=EDGE_LOOP('',(#1518,#1519));
#680=EDGE_LOOP('',(#1520,#1521,#1522));
#681=EDGE_LOOP('',(#1523,#1524,#1525));
#682=EDGE_LOOP('',(#1526,#1527,#1528,#1529,#1530));
#683=EDGE_LOOP('',(#1531,#1532,#1533,#1534,#1535,#1536));
#684=EDGE_LOOP('',(#1537,#1538));
#685=EDGE_LOOP('',(#1539,#1540,#1541));
#686=EDGE_LOOP('',(#1542,#1543,#1544));
#687=EDGE_LOOP('',(#1545,#1546,#1547,#1548,#1549));
#688=EDGE_LOOP('',(#1550));
#689=EDGE_LOOP('',(#1551,#1552,#1553,#1554));
#690=EDGE_LOOP('',(#1555,#1556,#1557,#1558));
#691=EDGE_LOOP('',(#1559,#1560,#1561,#1562));
#692=EDGE_LOOP('',(#1563,#1564,#1565,#1566));
#693=EDGE_LOOP('',(#1567,#1568,#1569,#1570));
#694=EDGE_LOOP('',(#1571,#1572,#1573,#1574));
#695=EDGE_LOOP('',(#1575,#1576,#1577,#1578,#1579));
#696=EDGE_LOOP('',(#1580));
#697=EDGE_LOOP('',(#1581,#1582,#1583,#1584,#1585));
#698=EDGE_LOOP('',(#1586));
#699=EDGE_LOOP('',(#1587,#1588,#1589,#1590,#1591));
#700=EDGE_LOOP('',(#1592,#1593,#1594,#1595,#1596));
#701=EDGE_LOOP('',(#1597,#1598,#1599,#1600,#1601));
#702=EDGE_LOOP('',(#1602,#1603,#1604,#1605,#1606));
#703=EDGE_LOOP('',(#1607,#1608,#1609,#1610));
#704=EDGE_LOOP('',(#1611));
#705=EDGE_LOOP('',(#1612));
#706=EDGE_LOOP('',(#1613,#1614,#1615,#1616));
#707=EDGE_LOOP('',(#1617));
#708=EDGE_LOOP('',(#1618));
#709=EDGE_LOOP('',(#1619,#1620,#1621,#1622));
#710=EDGE_LOOP('',(#1623,#1624,#1625,#1626));
#711=EDGE_LOOP('',(#1627,#1628,#1629,#1630));
#712=EDGE_LOOP('',(#1631,#1632,#1633,#1634));
#713=EDGE_LOOP('',(#1635,#1636,#1637,#1638));
#714=EDGE_LOOP('',(#1639,#1640,#1641,#1642));
#715=EDGE_LOOP('',(#1643,#1644,#1645,#1646));
#716=EDGE_LOOP('',(#1647,#1648,#1649,#1650));
#717=EDGE_LOOP('',(#1651,#1652,#1653,#1654));
#718=EDGE_LOOP('',(#1655,#1656,#1657,#1658));
#719=EDGE_LOOP('',(#1659,#1660,#1661,#1662));
#720=EDGE_LOOP('',(#1663,#1664,#1665,#1666));
#721=EDGE_LOOP('',(#1667));
#722=EDGE_LOOP('',(#1668));
#723=EDGE_LOOP('',(#1669));
#724=EDGE_LOOP('',(#1670));
#725=EDGE_LOOP('',(#1671,#1672,#1673,#1674));
#726=EDGE_LOOP('',(#1675,#1676,#1677,#1678));
#727=EDGE_LOOP('',(#1679,#1680,#1681,#1682));
#728=EDGE_LOOP('',(#1683));
#729=EDGE_LOOP('',(#1684));
#730=EDGE_LOOP('',(#1685,#1686,#1687,#1688));
#731=EDGE_LOOP('',(#1689));
#732=EDGE_LOOP('',(#1690));
#733=EDGE_LOOP('',(#1691,#1692,#1693,#1694));
#734=EDGE_LOOP('',(#1695,#1696,#1697,#1698));
#735=EDGE_LOOP('',(#1699,#1700,#1701,#1702));
#736=EDGE_LOOP('',(#1703,#1704,#1705,#1706));
#737=CIRCLE('',#1964,2.);
#738=CIRCLE('',#1965,2.);
#739=CIRCLE('',#1966,0.5);
#740=CIRCLE('',#1967,2.5);
#741=CIRCLE('',#1969,2.);
#742=CIRCLE('',#1970,2.);
#743=CIRCLE('',#1971,0.5);
#744=CIRCLE('',#1972,2.5);
#745=CIRCLE('',#1974,2.);
#746=CIRCLE('',#1976,2.);
#747=CIRCLE('',#1978,11.7723008899906);
#748=CIRCLE('',#1979,11.7723008899906);
#749=CIRCLE('',#1981,12.2723008899906);
#750=CIRCLE('',#1982,12.2723008899906);
#751=CIRCLE('',#1984,12.2723008899906);
#752=CIRCLE('',#1987,12.2723008899906);
#753=CIRCLE('',#1990,0.5);
#754=CIRCLE('',#1991,0.5);
#755=CIRCLE('',#1993,0.5);
#756=CIRCLE('',#1995,0.5);
#757=CIRCLE('',#1999,2.);
#758=CIRCLE('',#2000,2.);
#759=CIRCLE('',#2007,2.00000000000001);
#760=CIRCLE('',#2008,2.00000000000001);
#761=CIRCLE('',#2016,1.);
#762=CIRCLE('',#2017,1.);
#763=CIRCLE('',#2024,2.00000000000001);
#764=CIRCLE('',#2025,2.00000000000001);
#765=CIRCLE('',#2027,1.);
#766=CIRCLE('',#2028,1.);
#767=CIRCLE('',#2029,3471.58024051075);
#768=CIRCLE('',#2038,1.);
#769=CIRCLE('',#2039,1.);
#770=CIRCLE('',#2041,1.5);
#771=CIRCLE('',#2042,1.5);
#772=CIRCLE('',#2051,0.250000000000001);
#773=CIRCLE('',#2052,0.250000000000001);
#774=CIRCLE('',#2053,1.74999999999999);
#775=CIRCLE('',#2054,0.249999999999999);
#776=CIRCLE('',#2056,0.25);
#777=CIRCLE('',#2057,0.3);
#778=CIRCLE('',#2058,0.300000000000001);
#779=CIRCLE('',#2059,0.300000000000001);
#780=CIRCLE('',#2060,0.299999999999999);
#781=CIRCLE('',#2063,0.299999999999999);
#782=CIRCLE('',#2066,0.300000000000001);
#783=CIRCLE('',#2067,0.300000000000001);
#784=CIRCLE('',#2068,0.3);
#785=CIRCLE('',#2072,0.25);
#786=CIRCLE('',#2076,2.00000000000001);
#787=CIRCLE('',#2077,2.00000000000001);
#788=CIRCLE('',#2082,2.);
#789=CIRCLE('',#2083,2.);
#790=CIRCLE('',#2084,0.5);
#791=CIRCLE('',#2085,2.5);
#792=CIRCLE('',#2087,2.);
#793=CIRCLE('',#2088,2.);
#794=CIRCLE('',#2089,0.5);
#795=CIRCLE('',#2090,2.5);
#796=CIRCLE('',#2092,2.);
#797=CIRCLE('',#2094,2.);
#798=CIRCLE('',#2096,11.7723008899906);
#799=CIRCLE('',#2097,11.7723008899906);
#800=CIRCLE('',#2099,12.2723008899906);
#801=CIRCLE('',#2100,12.2723008899906);
#802=CIRCLE('',#2102,12.2723008899906);
#803=CIRCLE('',#2105,12.2723008899906);
#804=CIRCLE('',#2108,0.5);
#805=CIRCLE('',#2109,0.5);
#806=CIRCLE('',#2111,0.5);
#807=CIRCLE('',#2113,0.5);
#808=CIRCLE('',#2117,3.5);
#809=CIRCLE('',#2118,0.5);
#810=CIRCLE('',#2119,4.);
#811=CIRCLE('',#2121,4.);
#812=CIRCLE('',#2122,0.5);
#813=CIRCLE('',#2123,3.5);
#814=CIRCLE('',#2125,2.);
#815=CIRCLE('',#2126,2.);
#816=CIRCLE('',#2133,2.);
#817=CIRCLE('',#2134,2.);
#818=CIRCLE('',#2136,2.00000000000001);
#819=CIRCLE('',#2137,2.00000000000001);
#820=CIRCLE('',#2139,9.00000000000003);
#821=CIRCLE('',#2140,9.00000000000005);
#822=CIRCLE('',#2142,9.00000000000003);
#823=CIRCLE('',#2143,9.00000000000005);
#824=VERTEX_POINT('',#2655);
#825=VERTEX_POINT('',#2656);
#826=VERTEX_POINT('',#2659);
#827=VERTEX_POINT('',#2663);
#828=VERTEX_POINT('',#2664);
#829=VERTEX_POINT('',#2667);
#830=VERTEX_POINT('',#2671);
#831=VERTEX_POINT('',#2675);
#832=VERTEX_POINT('',#2679);
#833=VERTEX_POINT('',#2680);
#834=VERTEX_POINT('',#2682);
#835=VERTEX_POINT('',#2684);
#836=VERTEX_POINT('',#2688);
#837=VERTEX_POINT('',#2689);
#838=VERTEX_POINT('',#2691);
#839=VERTEX_POINT('',#2693);
#840=VERTEX_POINT('',#2697);
#841=VERTEX_POINT('',#2699);
#842=VERTEX_POINT('',#2703);
#843=VERTEX_POINT('',#2707);
#844=VERTEX_POINT('',#2722);
#845=VERTEX_POINT('',#2724);
#846=VERTEX_POINT('',#2751);
#847=VERTEX_POINT('',#2752);
#848=VERTEX_POINT('',#2765);
#849=VERTEX_POINT('',#2767);
#850=VERTEX_POINT('',#2793);
#851=VERTEX_POINT('',#2800);
#852=VERTEX_POINT('',#2822);
#853=VERTEX_POINT('',#2830);
#854=VERTEX_POINT('',#2846);
#855=VERTEX_POINT('',#3178);
#856=VERTEX_POINT('',#3182);
#857=VERTEX_POINT('',#3184);
#858=VERTEX_POINT('',#3620);
#859=VERTEX_POINT('',#3622);
#860=VERTEX_POINT('',#3641);
#861=VERTEX_POINT('',#3642);
#862=VERTEX_POINT('',#3644);
#863=VERTEX_POINT('',#3653);
#864=VERTEX_POINT('',#3687);
#865=VERTEX_POINT('',#3688);
#866=VERTEX_POINT('',#3697);
#867=VERTEX_POINT('',#3831);
#868=VERTEX_POINT('',#3833);
#869=VERTEX_POINT('',#3859);
#870=VERTEX_POINT('',#3866);
#871=VERTEX_POINT('',#3888);
#872=VERTEX_POINT('',#4297);
#873=VERTEX_POINT('',#4301);
#874=VERTEX_POINT('',#4595);
#875=VERTEX_POINT('',#4597);
#876=VERTEX_POINT('',#4606);
#877=VERTEX_POINT('',#4607);
#878=VERTEX_POINT('',#4609);
#879=VERTEX_POINT('',#4666);
#880=VERTEX_POINT('',#4683);
#881=VERTEX_POINT('',#4697);
#882=VERTEX_POINT('',#4703);
#883=VERTEX_POINT('',#4734);
#884=VERTEX_POINT('',#4735);
#885=VERTEX_POINT('',#4737);
#886=VERTEX_POINT('',#4750);
#887=VERTEX_POINT('',#4770);
#888=VERTEX_POINT('',#4774);
#889=VERTEX_POINT('',#4780);
#890=VERTEX_POINT('',#5023);
#891=VERTEX_POINT('',#5025);
#892=VERTEX_POINT('',#5029);
#893=VERTEX_POINT('',#5031);
#894=VERTEX_POINT('',#5042);
#895=VERTEX_POINT('',#5043);
#896=VERTEX_POINT('',#5048);
#897=VERTEX_POINT('',#5056);
#898=VERTEX_POINT('',#5058);
#899=VERTEX_POINT('',#5070);
#900=VERTEX_POINT('',#5096);
#901=VERTEX_POINT('',#5129);
#902=VERTEX_POINT('',#5130);
#903=VERTEX_POINT('',#5146);
#904=VERTEX_POINT('',#5148);
#905=VERTEX_POINT('',#5169);
#906=VERTEX_POINT('',#5171);
#907=VERTEX_POINT('',#5175);
#908=VERTEX_POINT('',#5176);
#909=VERTEX_POINT('',#5184);
#910=VERTEX_POINT('',#5255);
#911=VERTEX_POINT('',#5257);
#912=VERTEX_POINT('',#5261);
#913=VERTEX_POINT('',#5263);
#914=VERTEX_POINT('',#5274);
#915=VERTEX_POINT('',#5275);
#916=VERTEX_POINT('',#5278);
#917=VERTEX_POINT('',#5365);
#918=VERTEX_POINT('',#5378);
#919=VERTEX_POINT('',#5380);
#920=VERTEX_POINT('',#5674);
#921=VERTEX_POINT('',#5675);
#922=VERTEX_POINT('',#5700);
#923=VERTEX_POINT('',#5747);
#924=VERTEX_POINT('',#5749);
#925=VERTEX_POINT('',#7721);
#926=VERTEX_POINT('',#7723);
#927=VERTEX_POINT('',#7917);
#928=VERTEX_POINT('',#7919);
#929=VERTEX_POINT('',#9937);
#930=VERTEX_POINT('',#9941);
#931=VERTEX_POINT('',#11680);
#932=VERTEX_POINT('',#11682);
#933=VERTEX_POINT('',#11773);
#934=VERTEX_POINT('',#11774);
#935=VERTEX_POINT('',#11819);
#936=VERTEX_POINT('',#11821);
#937=VERTEX_POINT('',#11877);
#938=VERTEX_POINT('',#11882);
#939=VERTEX_POINT('',#11900);
#940=VERTEX_POINT('',#11907);
#941=VERTEX_POINT('',#11925);
#942=VERTEX_POINT('',#11931);
#943=VERTEX_POINT('',#11970);
#944=VERTEX_POINT('',#11971);
#945=VERTEX_POINT('',#11974);
#946=VERTEX_POINT('',#11978);
#947=VERTEX_POINT('',#11979);
#948=VERTEX_POINT('',#11982);
#949=VERTEX_POINT('',#11986);
#950=VERTEX_POINT('',#11990);
#951=VERTEX_POINT('',#11994);
#952=VERTEX_POINT('',#11995);
#953=VERTEX_POINT('',#11997);
#954=VERTEX_POINT('',#11999);
#955=VERTEX_POINT('',#12003);
#956=VERTEX_POINT('',#12004);
#957=VERTEX_POINT('',#12006);
#958=VERTEX_POINT('',#12008);
#959=VERTEX_POINT('',#12012);
#960=VERTEX_POINT('',#12014);
#961=VERTEX_POINT('',#12018);
#962=VERTEX_POINT('',#12022);
#963=VERTEX_POINT('',#12037);
#964=VERTEX_POINT('',#12039);
#965=VERTEX_POINT('',#12043);
#966=VERTEX_POINT('',#12045);
#967=VERTEX_POINT('',#12049);
#968=VERTEX_POINT('',#12051);
#969=VERTEX_POINT('',#12061);
#970=VERTEX_POINT('',#12063);
#971=VERTEX_POINT('',#12067);
#972=VERTEX_POINT('',#12069);
#973=VERTEX_POINT('',#12073);
#974=VERTEX_POINT('',#12074);
#975=VERTEX_POINT('',#12076);
#976=VERTEX_POINT('',#12078);
#977=VERTEX_POINT('',#12082);
#978=VERTEX_POINT('',#12083);
#979=VERTEX_POINT('',#12085);
#980=VERTEX_POINT('',#12087);
#981=EDGE_CURVE('',#824,#825,#737,.T.);
#982=EDGE_CURVE('',#825,#824,#738,.T.);
#983=EDGE_CURVE('',#825,#826,#739,.T.);
#984=EDGE_CURVE('',#826,#826,#740,.T.);
#985=EDGE_CURVE('',#827,#828,#741,.T.);
#986=EDGE_CURVE('',#828,#827,#742,.T.);
#987=EDGE_CURVE('',#828,#829,#743,.T.);
#988=EDGE_CURVE('',#829,#829,#744,.T.);
#989=EDGE_CURVE('',#827,#830,#276,.T.);
#990=EDGE_CURVE('',#830,#830,#745,.T.);
#991=EDGE_CURVE('',#824,#831,#277,.T.);
#992=EDGE_CURVE('',#831,#831,#746,.T.);
#993=EDGE_CURVE('',#832,#833,#747,.T.);
#994=EDGE_CURVE('',#833,#834,#278,.T.);
#995=EDGE_CURVE('',#834,#835,#748,.T.);
#996=EDGE_CURVE('',#835,#832,#279,.T.);
#997=EDGE_CURVE('',#836,#837,#749,.T.);
#998=EDGE_CURVE('',#838,#836,#280,.T.);
#999=EDGE_CURVE('',#839,#838,#750,.T.);
#1000=EDGE_CURVE('',#837,#839,#281,.T.);
#1001=EDGE_CURVE('',#840,#837,#282,.T.);
#1002=EDGE_CURVE('',#840,#841,#751,.T.);
#1003=EDGE_CURVE('',#841,#836,#283,.T.);
#1004=EDGE_CURVE('',#842,#839,#284,.T.);
#1005=EDGE_CURVE('',#842,#840,#285,.T.);
#1006=EDGE_CURVE('',#843,#838,#286,.T.);
#1007=EDGE_CURVE('',#843,#842,#752,.T.);
#1008=EDGE_CURVE('',#841,#843,#287,.T.);
#1009=EDGE_CURVE('',#840,#835,#753,.T.);
#1010=EDGE_CURVE('',#832,#842,#754,.T.);
#1011=EDGE_CURVE('',#833,#843,#755,.T.);
#1012=EDGE_CURVE('',#841,#834,#756,.T.);
#1013=EDGE_CURVE('',#844,#844,#757,.T.);
#1014=EDGE_CURVE('',#844,#845,#288,.T.);
#1015=EDGE_CURVE('',#845,#845,#758,.T.);
#1016=EDGE_CURVE('',#846,#847,#81,.T.);
#1017=EDGE_CURVE('',#848,#846,#289,.T.);
#1018=EDGE_CURVE('',#848,#849,#82,.T.);
#1019=EDGE_CURVE('',#847,#849,#290,.T.);
#1020=EDGE_CURVE('',#849,#850,#83,.T.);
#1021=EDGE_CURVE('',#851,#850,#291,.T.);
#1022=EDGE_CURVE('',#847,#851,#84,.T.);
#1023=EDGE_CURVE('',#850,#852,#85,.T.);
#1024=EDGE_CURVE('',#852,#853,#86,.T.);
#1025=EDGE_CURVE('',#851,#853,#87,.T.);
#1026=EDGE_CURVE('',#853,#854,#88,.T.);
#1027=EDGE_CURVE('',#855,#854,#292,.T.);
#1028=EDGE_CURVE('',#846,#855,#293,.T.);
#1029=EDGE_CURVE('',#848,#856,#294,.T.);
#1030=EDGE_CURVE('',#856,#857,#295,.T.);
#1031=EDGE_CURVE('',#852,#857,#89,.T.);
#1032=EDGE_CURVE('',#854,#857,#90,.T.);
#1033=EDGE_CURVE('',#856,#855,#296,.T.);
#1034=EDGE_CURVE('',#858,#858,#759,.T.);
#1035=EDGE_CURVE('',#858,#859,#297,.T.);
#1036=EDGE_CURVE('',#859,#859,#760,.T.);
#1037=EDGE_CURVE('',#860,#861,#298,.T.);
#1038=EDGE_CURVE('',#861,#862,#91,.T.);
#1039=EDGE_CURVE('',#862,#863,#299,.T.);
#1040=EDGE_CURVE('',#863,#860,#92,.T.);
#1041=EDGE_CURVE('',#864,#865,#93,.T.);
#1042=EDGE_CURVE('',#864,#866,#94,.T.);
#1043=EDGE_CURVE('',#867,#866,#300,.T.);
#1044=EDGE_CURVE('',#867,#868,#95,.T.);
#1045=EDGE_CURVE('',#865,#868,#301,.T.);
#1046=EDGE_CURVE('',#868,#869,#96,.T.);
#1047=EDGE_CURVE('',#870,#869,#302,.T.);
#1048=EDGE_CURVE('',#865,#870,#97,.T.);
#1049=EDGE_CURVE('',#862,#871,#98,.T.);
#1050=EDGE_CURVE('',#870,#871,#99,.T.);
#1051=EDGE_CURVE('',#869,#863,#100,.T.);
#1052=EDGE_CURVE('',#871,#864,#101,.T.);
#1053=EDGE_CURVE('',#872,#860,#303,.T.);
#1054=EDGE_CURVE('',#867,#872,#304,.T.);
#1055=EDGE_CURVE('',#872,#873,#305,.T.);
#1056=EDGE_CURVE('',#873,#861,#306,.T.);
#1057=EDGE_CURVE('',#866,#873,#102,.T.);
#1058=EDGE_CURVE('',#874,#874,#761,.T.);
#1059=EDGE_CURVE('',#874,#875,#307,.T.);
#1060=EDGE_CURVE('',#875,#875,#762,.T.);
#1061=EDGE_CURVE('',#876,#877,#308,.T.);
#1062=EDGE_CURVE('',#877,#878,#103,.T.);
#1063=EDGE_CURVE('',#879,#878,#309,.T.);
#1064=EDGE_CURVE('',#876,#879,#104,.T.);
#1065=EDGE_CURVE('',#878,#880,#105,.T.);
#1066=EDGE_CURVE('',#880,#881,#106,.T.);
#1067=EDGE_CURVE('',#882,#881,#310,.T.);
#1068=EDGE_CURVE('',#879,#882,#107,.T.);
#1069=EDGE_CURVE('',#883,#884,#311,.T.);
#1070=EDGE_CURVE('',#885,#883,#108,.T.);
#1071=EDGE_CURVE('',#885,#886,#312,.T.);
#1072=EDGE_CURVE('',#886,#884,#109,.T.);
#1073=EDGE_CURVE('',#884,#887,#110,.T.);
#1074=EDGE_CURVE('',#888,#887,#313,.T.);
#1075=EDGE_CURVE('',#883,#888,#111,.T.);
#1076=EDGE_CURVE('',#887,#889,#314,.T.);
#1077=EDGE_CURVE('',#889,#877,#112,.T.);
#1078=EDGE_CURVE('',#888,#876,#315,.T.);
#1079=EDGE_CURVE('',#885,#882,#316,.T.);
#1080=EDGE_CURVE('',#880,#889,#113,.T.);
#1081=EDGE_CURVE('',#881,#886,#317,.T.);
#1082=EDGE_CURVE('',#890,#890,#763,.T.);
#1083=EDGE_CURVE('',#890,#891,#318,.T.);
#1084=EDGE_CURVE('',#891,#891,#764,.T.);
#1085=EDGE_CURVE('',#892,#892,#765,.T.);
#1086=EDGE_CURVE('',#892,#893,#319,.T.);
#1087=EDGE_CURVE('',#893,#893,#766,.T.);
#1088=EDGE_CURVE('',#894,#895,#114,.T.);
#1089=EDGE_CURVE('',#895,#896,#115,.T.);
#1090=EDGE_CURVE('',#897,#896,#320,.T.);
#1091=EDGE_CURVE('',#898,#897,#116,.T.);
#1092=EDGE_CURVE('',#898,#894,#321,.T.);
#1093=EDGE_CURVE('',#896,#899,#117,.T.);
#1094=EDGE_CURVE('',#900,#899,#322,.T.);
#1095=EDGE_CURVE('',#897,#900,#767,.T.);
#1096=EDGE_CURVE('',#901,#902,#118,.T.);
#1097=EDGE_CURVE('',#903,#902,#323,.T.);
#1098=EDGE_CURVE('',#904,#903,#119,.T.);
#1099=EDGE_CURVE('',#904,#901,#324,.T.);
#1100=EDGE_CURVE('',#902,#894,#325,.T.);
#1101=EDGE_CURVE('',#903,#898,#326,.T.);
#1102=EDGE_CURVE('',#905,#900,#327,.T.);
#1103=EDGE_CURVE('',#906,#905,#328,.T.);
#1104=EDGE_CURVE('',#906,#904,#329,.T.);
#1105=EDGE_CURVE('',#907,#908,#330,.T.);
#1106=EDGE_CURVE('',#908,#895,#120,.T.);
#1107=EDGE_CURVE('',#909,#901,#331,.T.);
#1108=EDGE_CURVE('',#907,#909,#332,.T.);
#1109=EDGE_CURVE('',#899,#908,#333,.T.);
#1110=EDGE_CURVE('',#905,#907,#334,.T.);
#1111=EDGE_CURVE('',#909,#906,#335,.T.);
#1112=EDGE_CURVE('',#910,#910,#768,.T.);
#1113=EDGE_CURVE('',#910,#911,#336,.T.);
#1114=EDGE_CURVE('',#911,#911,#769,.T.);
#1115=EDGE_CURVE('',#912,#912,#770,.T.);
#1116=EDGE_CURVE('',#912,#913,#337,.T.);
#1117=EDGE_CURVE('',#913,#913,#771,.T.);
#1118=EDGE_CURVE('',#914,#915,#772,.T.);
#1119=EDGE_CURVE('',#915,#914,#773,.T.);
#1120=EDGE_CURVE('',#914,#916,#774,.T.);
#1121=EDGE_CURVE('',#916,#916,#775,.T.);
#1122=EDGE_CURVE('',#915,#917,#121,.T.);
#1123=EDGE_CURVE('',#917,#918,#12,.T.);
#1124=EDGE_CURVE('',#918,#919,#776,.T.);
#1125=EDGE_CURVE('',#914,#919,#122,.T.);
#1126=EDGE_CURVE('',#920,#921,#123,.T.);
#1127=EDGE_CURVE('',#921,#922,#124,.T.);
#1128=EDGE_CURVE('',#923,#922,#777,.T.);
#1129=EDGE_CURVE('',#924,#923,#125,.T.);
#1130=EDGE_CURVE('',#924,#920,#778,.T.);
#1131=EDGE_CURVE('',#920,#925,#779,.T.);
#1132=EDGE_CURVE('',#925,#926,#11,.T.);
#1133=EDGE_CURVE('',#926,#927,#780,.T.);
#1134=EDGE_CURVE('',#928,#927,#126,.T.);
#1135=EDGE_CURVE('',#921,#928,#13,.T.);
#1136=EDGE_CURVE('',#927,#926,#781,.T.);
#1137=EDGE_CURVE('',#918,#929,#338,.T.);
#1138=EDGE_CURVE('',#929,#917,#14,.T.);
#1139=EDGE_CURVE('',#920,#930,#339,.T.);
#1140=EDGE_CURVE('',#925,#930,#782,.T.);
#1141=EDGE_CURVE('',#928,#930,#127,.T.);
#1142=EDGE_CURVE('',#930,#924,#783,.T.);
#1143=EDGE_CURVE('',#922,#923,#784,.T.);
#1144=EDGE_CURVE('',#919,#929,#785,.T.);
#1145=EDGE_CURVE('',#931,#931,#786,.T.);
#1146=EDGE_CURVE('',#931,#932,#340,.T.);
#1147=EDGE_CURVE('',#932,#932,#787,.T.);
#1148=EDGE_CURVE('',#933,#934,#128,.T.);
#1149=EDGE_CURVE('',#935,#934,#341,.T.);
#1150=EDGE_CURVE('',#936,#935,#129,.T.);
#1151=EDGE_CURVE('',#936,#933,#342,.T.);
#1152=EDGE_CURVE('',#934,#937,#130,.T.);
#1153=EDGE_CURVE('',#938,#937,#343,.T.);
#1154=EDGE_CURVE('',#935,#938,#131,.T.);
#1155=EDGE_CURVE('',#937,#939,#132,.T.);
#1156=EDGE_CURVE('',#940,#939,#344,.T.);
#1157=EDGE_CURVE('',#938,#940,#133,.T.);
#1158=EDGE_CURVE('',#939,#941,#134,.T.);
#1159=EDGE_CURVE('',#942,#941,#345,.T.);
#1160=EDGE_CURVE('',#940,#942,#135,.T.);
#1161=EDGE_CURVE('',#941,#933,#136,.T.);
#1162=EDGE_CURVE('',#942,#936,#137,.T.);
#1163=EDGE_CURVE('',#943,#944,#788,.T.);
#1164=EDGE_CURVE('',#944,#943,#789,.T.);
#1165=EDGE_CURVE('',#944,#945,#790,.T.);
#1166=EDGE_CURVE('',#945,#945,#791,.T.);
#1167=EDGE_CURVE('',#946,#947,#792,.T.);
#1168=EDGE_CURVE('',#947,#946,#793,.T.);
#1169=EDGE_CURVE('',#947,#948,#794,.T.);
#1170=EDGE_CURVE('',#948,#948,#795,.T.);
#1171=EDGE_CURVE('',#946,#949,#346,.T.);
#1172=EDGE_CURVE('',#949,#949,#796,.T.);
#1173=EDGE_CURVE('',#943,#950,#347,.T.);
#1174=EDGE_CURVE('',#950,#950,#797,.T.);
#1175=EDGE_CURVE('',#951,#952,#798,.T.);
#1176=EDGE_CURVE('',#952,#953,#348,.T.);
#1177=EDGE_CURVE('',#953,#954,#799,.T.);
#1178=EDGE_CURVE('',#954,#951,#349,.T.);
#1179=EDGE_CURVE('',#955,#956,#800,.T.);
#1180=EDGE_CURVE('',#957,#955,#350,.T.);
#1181=EDGE_CURVE('',#958,#957,#801,.T.);
#1182=EDGE_CURVE('',#956,#958,#351,.T.);
#1183=EDGE_CURVE('',#959,#956,#352,.T.);
#1184=EDGE_CURVE('',#959,#960,#802,.T.);
#1185=EDGE_CURVE('',#960,#955,#353,.T.);
#1186=EDGE_CURVE('',#961,#958,#354,.T.);
#1187=EDGE_CURVE('',#961,#959,#355,.T.);
#1188=EDGE_CURVE('',#962,#957,#356,.T.);
#1189=EDGE_CURVE('',#962,#961,#803,.T.);
#1190=EDGE_CURVE('',#960,#962,#357,.T.);
#1191=EDGE_CURVE('',#959,#954,#804,.T.);
#1192=EDGE_CURVE('',#951,#961,#805,.T.);
#1193=EDGE_CURVE('',#952,#962,#806,.T.);
#1194=EDGE_CURVE('',#960,#953,#807,.T.);
#1195=EDGE_CURVE('',#963,#963,#808,.T.);
#1196=EDGE_CURVE('',#963,#964,#809,.T.);
#1197=EDGE_CURVE('',#964,#964,#810,.T.);
#1198=EDGE_CURVE('',#965,#965,#811,.T.);
#1199=EDGE_CURVE('',#965,#966,#812,.T.);
#1200=EDGE_CURVE('',#966,#966,#813,.T.);
#1201=EDGE_CURVE('',#967,#967,#814,.T.);
#1202=EDGE_CURVE('',#967,#968,#358,.T.);
#1203=EDGE_CURVE('',#968,#968,#815,.T.);
#1204=EDGE_CURVE('',#964,#965,#359,.T.);
#1205=EDGE_CURVE('',#969,#969,#816,.T.);
#1206=EDGE_CURVE('',#969,#970,#360,.T.);
#1207=EDGE_CURVE('',#970,#970,#817,.T.);
#1208=EDGE_CURVE('',#971,#971,#818,.T.);
#1209=EDGE_CURVE('',#971,#972,#361,.T.);
#1210=EDGE_CURVE('',#972,#972,#819,.T.);
#1211=EDGE_CURVE('',#973,#974,#820,.T.);
#1212=EDGE_CURVE('',#974,#975,#362,.T.);
#1213=EDGE_CURVE('',#975,#976,#821,.T.);
#1214=EDGE_CURVE('',#976,#973,#363,.T.);
#1215=EDGE_CURVE('',#977,#978,#822,.T.);
#1216=EDGE_CURVE('',#979,#977,#364,.T.);
#1217=EDGE_CURVE('',#980,#979,#823,.T.);
#1218=EDGE_CURVE('',#978,#980,#365,.T.);
#1219=EDGE_CURVE('',#974,#978,#366,.T.);
#1220=EDGE_CURVE('',#973,#977,#367,.T.);
#1221=EDGE_CURVE('',#975,#980,#368,.T.);
#1222=EDGE_CURVE('',#976,#979,#369,.T.);
#1223=ORIENTED_EDGE('',*,*,#981,.F.);
#1224=ORIENTED_EDGE('',*,*,#982,.F.);
#1225=ORIENTED_EDGE('',*,*,#983,.T.);
#1226=ORIENTED_EDGE('',*,*,#984,.F.);
#1227=ORIENTED_EDGE('',*,*,#983,.F.);
#1228=ORIENTED_EDGE('',*,*,#985,.F.);
#1229=ORIENTED_EDGE('',*,*,#986,.F.);
#1230=ORIENTED_EDGE('',*,*,#987,.T.);
#1231=ORIENTED_EDGE('',*,*,#988,.F.);
#1232=ORIENTED_EDGE('',*,*,#987,.F.);
#1233=ORIENTED_EDGE('',*,*,#985,.T.);
#1234=ORIENTED_EDGE('',*,*,#986,.T.);
#1235=ORIENTED_EDGE('',*,*,#989,.T.);
#1236=ORIENTED_EDGE('',*,*,#990,.F.);
#1237=ORIENTED_EDGE('',*,*,#989,.F.);
#1238=ORIENTED_EDGE('',*,*,#981,.T.);
#1239=ORIENTED_EDGE('',*,*,#982,.T.);
#1240=ORIENTED_EDGE('',*,*,#991,.T.);
#1241=ORIENTED_EDGE('',*,*,#992,.F.);
#1242=ORIENTED_EDGE('',*,*,#991,.F.);
#1243=ORIENTED_EDGE('',*,*,#993,.T.);
#1244=ORIENTED_EDGE('',*,*,#994,.T.);
#1245=ORIENTED_EDGE('',*,*,#995,.T.);
#1246=ORIENTED_EDGE('',*,*,#996,.T.);
#1247=ORIENTED_EDGE('',*,*,#984,.T.);
#1248=ORIENTED_EDGE('',*,*,#988,.T.);
#1249=ORIENTED_EDGE('',*,*,#997,.F.);
#1250=ORIENTED_EDGE('',*,*,#998,.F.);
#1251=ORIENTED_EDGE('',*,*,#999,.F.);
#1252=ORIENTED_EDGE('',*,*,#1000,.F.);
#1253=ORIENTED_EDGE('',*,*,#992,.T.);
#1254=ORIENTED_EDGE('',*,*,#990,.T.);
#1255=ORIENTED_EDGE('',*,*,#1001,.F.);
#1256=ORIENTED_EDGE('',*,*,#1002,.T.);
#1257=ORIENTED_EDGE('',*,*,#1003,.T.);
#1258=ORIENTED_EDGE('',*,*,#997,.T.);
#1259=ORIENTED_EDGE('',*,*,#1004,.F.);
#1260=ORIENTED_EDGE('',*,*,#1005,.T.);
#1261=ORIENTED_EDGE('',*,*,#1001,.T.);
#1262=ORIENTED_EDGE('',*,*,#1000,.T.);
#1263=ORIENTED_EDGE('',*,*,#1006,.F.);
#1264=ORIENTED_EDGE('',*,*,#1007,.T.);
#1265=ORIENTED_EDGE('',*,*,#1004,.T.);
#1266=ORIENTED_EDGE('',*,*,#999,.T.);
#1267=ORIENTED_EDGE('',*,*,#1003,.F.);
#1268=ORIENTED_EDGE('',*,*,#1008,.T.);
#1269=ORIENTED_EDGE('',*,*,#1006,.T.);
#1270=ORIENTED_EDGE('',*,*,#998,.T.);
#1271=ORIENTED_EDGE('',*,*,#1009,.F.);
#1272=ORIENTED_EDGE('',*,*,#1005,.F.);
#1273=ORIENTED_EDGE('',*,*,#1010,.F.);
#1274=ORIENTED_EDGE('',*,*,#996,.F.);
#1275=ORIENTED_EDGE('',*,*,#1010,.T.);
#1276=ORIENTED_EDGE('',*,*,#1007,.F.);
#1277=ORIENTED_EDGE('',*,*,#1011,.F.);
#1278=ORIENTED_EDGE('',*,*,#993,.F.);
#1279=ORIENTED_EDGE('',*,*,#1009,.T.);
#1280=ORIENTED_EDGE('',*,*,#995,.F.);
#1281=ORIENTED_EDGE('',*,*,#1012,.F.);
#1282=ORIENTED_EDGE('',*,*,#1002,.F.);
#1283=ORIENTED_EDGE('',*,*,#1011,.T.);
#1284=ORIENTED_EDGE('',*,*,#1008,.F.);
#1285=ORIENTED_EDGE('',*,*,#1012,.T.);
#1286=ORIENTED_EDGE('',*,*,#994,.F.);
#1287=ORIENTED_EDGE('',*,*,#1013,.T.);
#1288=ORIENTED_EDGE('',*,*,#1014,.T.);
#1289=ORIENTED_EDGE('',*,*,#1015,.T.);
#1290=ORIENTED_EDGE('',*,*,#1014,.F.);
#1291=ORIENTED_EDGE('',*,*,#1016,.F.);
#1292=ORIENTED_EDGE('',*,*,#1017,.F.);
#1293=ORIENTED_EDGE('',*,*,#1018,.T.);
#1294=ORIENTED_EDGE('',*,*,#1019,.F.);
#1295=ORIENTED_EDGE('',*,*,#1020,.T.);
#1296=ORIENTED_EDGE('',*,*,#1021,.F.);
#1297=ORIENTED_EDGE('',*,*,#1022,.F.);
#1298=ORIENTED_EDGE('',*,*,#1019,.T.);
#1299=ORIENTED_EDGE('',*,*,#1023,.T.);
#1300=ORIENTED_EDGE('',*,*,#1024,.T.);
#1301=ORIENTED_EDGE('',*,*,#1025,.F.);
#1302=ORIENTED_EDGE('',*,*,#1021,.T.);
#1303=ORIENTED_EDGE('',*,*,#1025,.T.);
#1304=ORIENTED_EDGE('',*,*,#1026,.T.);
#1305=ORIENTED_EDGE('',*,*,#1027,.F.);
#1306=ORIENTED_EDGE('',*,*,#1028,.F.);
#1307=ORIENTED_EDGE('',*,*,#1016,.T.);
#1308=ORIENTED_EDGE('',*,*,#1022,.T.);
#1309=ORIENTED_EDGE('',*,*,#1015,.F.);
#1310=ORIENTED_EDGE('',*,*,#1029,.T.);
#1311=ORIENTED_EDGE('',*,*,#1030,.T.);
#1312=ORIENTED_EDGE('',*,*,#1031,.F.);
#1313=ORIENTED_EDGE('',*,*,#1023,.F.);
#1314=ORIENTED_EDGE('',*,*,#1020,.F.);
#1315=ORIENTED_EDGE('',*,*,#1018,.F.);
#1316=ORIENTED_EDGE('',*,*,#1013,.F.);
#1317=ORIENTED_EDGE('',*,*,#1027,.T.);
#1318=ORIENTED_EDGE('',*,*,#1032,.T.);
#1319=ORIENTED_EDGE('',*,*,#1030,.F.);
#1320=ORIENTED_EDGE('',*,*,#1033,.T.);
#1321=ORIENTED_EDGE('',*,*,#1028,.T.);
#1322=ORIENTED_EDGE('',*,*,#1033,.F.);
#1323=ORIENTED_EDGE('',*,*,#1029,.F.);
#1324=ORIENTED_EDGE('',*,*,#1017,.T.);
#1325=ORIENTED_EDGE('',*,*,#1024,.F.);
#1326=ORIENTED_EDGE('',*,*,#1031,.T.);
#1327=ORIENTED_EDGE('',*,*,#1032,.F.);
#1328=ORIENTED_EDGE('',*,*,#1026,.F.);
#1329=ORIENTED_EDGE('',*,*,#1034,.F.);
#1330=ORIENTED_EDGE('',*,*,#1035,.T.);
#1331=ORIENTED_EDGE('',*,*,#1036,.T.);
#1332=ORIENTED_EDGE('',*,*,#1035,.F.);
#1333=ORIENTED_EDGE('',*,*,#1037,.T.);
#1334=ORIENTED_EDGE('',*,*,#1038,.T.);
#1335=ORIENTED_EDGE('',*,*,#1039,.T.);
#1336=ORIENTED_EDGE('',*,*,#1040,.T.);
#1337=ORIENTED_EDGE('',*,*,#1041,.F.);
#1338=ORIENTED_EDGE('',*,*,#1042,.T.);
#1339=ORIENTED_EDGE('',*,*,#1043,.F.);
#1340=ORIENTED_EDGE('',*,*,#1044,.T.);
#1341=ORIENTED_EDGE('',*,*,#1045,.F.);
#1342=ORIENTED_EDGE('',*,*,#1046,.T.);
#1343=ORIENTED_EDGE('',*,*,#1047,.F.);
#1344=ORIENTED_EDGE('',*,*,#1048,.F.);
#1345=ORIENTED_EDGE('',*,*,#1045,.T.);
#1346=ORIENTED_EDGE('',*,*,#1039,.F.);
#1347=ORIENTED_EDGE('',*,*,#1049,.T.);
#1348=ORIENTED_EDGE('',*,*,#1050,.F.);
#1349=ORIENTED_EDGE('',*,*,#1047,.T.);
#1350=ORIENTED_EDGE('',*,*,#1051,.T.);
#1351=ORIENTED_EDGE('',*,*,#1050,.T.);
#1352=ORIENTED_EDGE('',*,*,#1052,.T.);
#1353=ORIENTED_EDGE('',*,*,#1041,.T.);
#1354=ORIENTED_EDGE('',*,*,#1048,.T.);
#1355=ORIENTED_EDGE('',*,*,#1036,.F.);
#1356=ORIENTED_EDGE('',*,*,#1053,.T.);
#1357=ORIENTED_EDGE('',*,*,#1040,.F.);
#1358=ORIENTED_EDGE('',*,*,#1051,.F.);
#1359=ORIENTED_EDGE('',*,*,#1046,.F.);
#1360=ORIENTED_EDGE('',*,*,#1044,.F.);
#1361=ORIENTED_EDGE('',*,*,#1054,.T.);
#1362=ORIENTED_EDGE('',*,*,#1034,.T.);
#1363=ORIENTED_EDGE('',*,*,#1055,.T.);
#1364=ORIENTED_EDGE('',*,*,#1056,.T.);
#1365=ORIENTED_EDGE('',*,*,#1037,.F.);
#1366=ORIENTED_EDGE('',*,*,#1053,.F.);
#1367=ORIENTED_EDGE('',*,*,#1043,.T.);
#1368=ORIENTED_EDGE('',*,*,#1057,.T.);
#1369=ORIENTED_EDGE('',*,*,#1055,.F.);
#1370=ORIENTED_EDGE('',*,*,#1054,.F.);
#1371=ORIENTED_EDGE('',*,*,#1042,.F.);
#1372=ORIENTED_EDGE('',*,*,#1052,.F.);
#1373=ORIENTED_EDGE('',*,*,#1049,.F.);
#1374=ORIENTED_EDGE('',*,*,#1038,.F.);
#1375=ORIENTED_EDGE('',*,*,#1056,.F.);
#1376=ORIENTED_EDGE('',*,*,#1057,.F.);
#1377=ORIENTED_EDGE('',*,*,#1058,.F.);
#1378=ORIENTED_EDGE('',*,*,#1059,.T.);
#1379=ORIENTED_EDGE('',*,*,#1060,.T.);
#1380=ORIENTED_EDGE('',*,*,#1059,.F.);
#1381=ORIENTED_EDGE('',*,*,#1061,.T.);
#1382=ORIENTED_EDGE('',*,*,#1062,.T.);
#1383=ORIENTED_EDGE('',*,*,#1063,.F.);
#1384=ORIENTED_EDGE('',*,*,#1064,.F.);
#1385=ORIENTED_EDGE('',*,*,#1063,.T.);
#1386=ORIENTED_EDGE('',*,*,#1065,.T.);
#1387=ORIENTED_EDGE('',*,*,#1066,.T.);
#1388=ORIENTED_EDGE('',*,*,#1067,.F.);
#1389=ORIENTED_EDGE('',*,*,#1068,.F.);
#1390=ORIENTED_EDGE('',*,*,#1069,.F.);
#1391=ORIENTED_EDGE('',*,*,#1070,.F.);
#1392=ORIENTED_EDGE('',*,*,#1071,.T.);
#1393=ORIENTED_EDGE('',*,*,#1072,.T.);
#1394=ORIENTED_EDGE('',*,*,#1073,.T.);
#1395=ORIENTED_EDGE('',*,*,#1074,.F.);
#1396=ORIENTED_EDGE('',*,*,#1075,.F.);
#1397=ORIENTED_EDGE('',*,*,#1069,.T.);
#1398=ORIENTED_EDGE('',*,*,#1076,.T.);
#1399=ORIENTED_EDGE('',*,*,#1077,.T.);
#1400=ORIENTED_EDGE('',*,*,#1061,.F.);
#1401=ORIENTED_EDGE('',*,*,#1078,.F.);
#1402=ORIENTED_EDGE('',*,*,#1074,.T.);
#1403=ORIENTED_EDGE('',*,*,#1068,.T.);
#1404=ORIENTED_EDGE('',*,*,#1079,.F.);
#1405=ORIENTED_EDGE('',*,*,#1070,.T.);
#1406=ORIENTED_EDGE('',*,*,#1075,.T.);
#1407=ORIENTED_EDGE('',*,*,#1078,.T.);
#1408=ORIENTED_EDGE('',*,*,#1064,.T.);
#1409=ORIENTED_EDGE('',*,*,#1060,.F.);
#1410=ORIENTED_EDGE('',*,*,#1066,.F.);
#1411=ORIENTED_EDGE('',*,*,#1080,.T.);
#1412=ORIENTED_EDGE('',*,*,#1076,.F.);
#1413=ORIENTED_EDGE('',*,*,#1073,.F.);
#1414=ORIENTED_EDGE('',*,*,#1072,.F.);
#1415=ORIENTED_EDGE('',*,*,#1081,.F.);
#1416=ORIENTED_EDGE('',*,*,#1058,.T.);
#1417=ORIENTED_EDGE('',*,*,#1079,.T.);
#1418=ORIENTED_EDGE('',*,*,#1067,.T.);
#1419=ORIENTED_EDGE('',*,*,#1081,.T.);
#1420=ORIENTED_EDGE('',*,*,#1071,.F.);
#1421=ORIENTED_EDGE('',*,*,#1077,.F.);
#1422=ORIENTED_EDGE('',*,*,#1080,.F.);
#1423=ORIENTED_EDGE('',*,*,#1065,.F.);
#1424=ORIENTED_EDGE('',*,*,#1062,.F.);
#1425=ORIENTED_EDGE('',*,*,#1082,.F.);
#1426=ORIENTED_EDGE('',*,*,#1083,.T.);
#1427=ORIENTED_EDGE('',*,*,#1084,.T.);
#1428=ORIENTED_EDGE('',*,*,#1083,.F.);
#1429=ORIENTED_EDGE('',*,*,#1085,.F.);
#1430=ORIENTED_EDGE('',*,*,#1086,.T.);
#1431=ORIENTED_EDGE('',*,*,#1087,.T.);
#1432=ORIENTED_EDGE('',*,*,#1086,.F.);
#1433=ORIENTED_EDGE('',*,*,#1088,.T.);
#1434=ORIENTED_EDGE('',*,*,#1089,.T.);
#1435=ORIENTED_EDGE('',*,*,#1090,.F.);
#1436=ORIENTED_EDGE('',*,*,#1091,.F.);
#1437=ORIENTED_EDGE('',*,*,#1092,.T.);
#1438=ORIENTED_EDGE('',*,*,#1090,.T.);
#1439=ORIENTED_EDGE('',*,*,#1093,.T.);
#1440=ORIENTED_EDGE('',*,*,#1094,.F.);
#1441=ORIENTED_EDGE('',*,*,#1095,.F.);
#1442=ORIENTED_EDGE('',*,*,#1096,.T.);
#1443=ORIENTED_EDGE('',*,*,#1097,.F.);
#1444=ORIENTED_EDGE('',*,*,#1098,.F.);
#1445=ORIENTED_EDGE('',*,*,#1099,.T.);
#1446=ORIENTED_EDGE('',*,*,#1100,.T.);
#1447=ORIENTED_EDGE('',*,*,#1092,.F.);
#1448=ORIENTED_EDGE('',*,*,#1101,.F.);
#1449=ORIENTED_EDGE('',*,*,#1097,.T.);
#1450=ORIENTED_EDGE('',*,*,#1091,.T.);
#1451=ORIENTED_EDGE('',*,*,#1095,.T.);
#1452=ORIENTED_EDGE('',*,*,#1102,.F.);
#1453=ORIENTED_EDGE('',*,*,#1103,.F.);
#1454=ORIENTED_EDGE('',*,*,#1104,.T.);
#1455=ORIENTED_EDGE('',*,*,#1098,.T.);
#1456=ORIENTED_EDGE('',*,*,#1101,.T.);
#1457=ORIENTED_EDGE('',*,*,#1084,.F.);
#1458=ORIENTED_EDGE('',*,*,#1087,.F.);
#1459=ORIENTED_EDGE('',*,*,#1105,.T.);
#1460=ORIENTED_EDGE('',*,*,#1106,.T.);
#1461=ORIENTED_EDGE('',*,*,#1088,.F.);
#1462=ORIENTED_EDGE('',*,*,#1100,.F.);
#1463=ORIENTED_EDGE('',*,*,#1096,.F.);
#1464=ORIENTED_EDGE('',*,*,#1107,.F.);
#1465=ORIENTED_EDGE('',*,*,#1108,.F.);
#1466=ORIENTED_EDGE('',*,*,#1082,.T.);
#1467=ORIENTED_EDGE('',*,*,#1085,.T.);
#1468=ORIENTED_EDGE('',*,*,#1094,.T.);
#1469=ORIENTED_EDGE('',*,*,#1109,.T.);
#1470=ORIENTED_EDGE('',*,*,#1105,.F.);
#1471=ORIENTED_EDGE('',*,*,#1110,.F.);
#1472=ORIENTED_EDGE('',*,*,#1102,.T.);
#1473=ORIENTED_EDGE('',*,*,#1099,.F.);
#1474=ORIENTED_EDGE('',*,*,#1104,.F.);
#1475=ORIENTED_EDGE('',*,*,#1111,.F.);
#1476=ORIENTED_EDGE('',*,*,#1107,.T.);
#1477=ORIENTED_EDGE('',*,*,#1103,.T.);
#1478=ORIENTED_EDGE('',*,*,#1110,.T.);
#1479=ORIENTED_EDGE('',*,*,#1108,.T.);
#1480=ORIENTED_EDGE('',*,*,#1111,.T.);
#1481=ORIENTED_EDGE('',*,*,#1089,.F.);
#1482=ORIENTED_EDGE('',*,*,#1106,.F.);
#1483=ORIENTED_EDGE('',*,*,#1109,.F.);
#1484=ORIENTED_EDGE('',*,*,#1093,.F.);
#1485=ORIENTED_EDGE('',*,*,#1112,.T.);
#1486=ORIENTED_EDGE('',*,*,#1113,.T.);
#1487=ORIENTED_EDGE('',*,*,#1114,.F.);
#1488=ORIENTED_EDGE('',*,*,#1113,.F.);
#1489=ORIENTED_EDGE('',*,*,#1115,.T.);
#1490=ORIENTED_EDGE('',*,*,#1116,.T.);
#1491=ORIENTED_EDGE('',*,*,#1117,.F.);
#1492=ORIENTED_EDGE('',*,*,#1116,.F.);
#1493=ORIENTED_EDGE('',*,*,#1117,.T.);
#1494=ORIENTED_EDGE('',*,*,#1112,.F.);
#1495=ORIENTED_EDGE('',*,*,#1115,.F.);
#1496=ORIENTED_EDGE('',*,*,#1114,.T.);
#1497=ORIENTED_EDGE('',*,*,#1118,.T.);
#1498=ORIENTED_EDGE('',*,*,#1119,.T.);
#1499=ORIENTED_EDGE('',*,*,#1120,.T.);
#1500=ORIENTED_EDGE('',*,*,#1121,.F.);
#1501=ORIENTED_EDGE('',*,*,#1120,.F.);
#1502=ORIENTED_EDGE('',*,*,#1119,.F.);
#1503=ORIENTED_EDGE('',*,*,#1122,.T.);
#1504=ORIENTED_EDGE('',*,*,#1123,.T.);
#1505=ORIENTED_EDGE('',*,*,#1124,.T.);
#1506=ORIENTED_EDGE('',*,*,#1125,.F.);
#1507=ORIENTED_EDGE('',*,*,#1126,.T.);
#1508=ORIENTED_EDGE('',*,*,#1127,.T.);
#1509=ORIENTED_EDGE('',*,*,#1128,.F.);
#1510=ORIENTED_EDGE('',*,*,#1129,.F.);
#1511=ORIENTED_EDGE('',*,*,#1130,.T.);
#1512=ORIENTED_EDGE('',*,*,#1131,.T.);
#1513=ORIENTED_EDGE('',*,*,#1132,.T.);
#1514=ORIENTED_EDGE('',*,*,#1133,.T.);
#1515=ORIENTED_EDGE('',*,*,#1134,.F.);
#1516=ORIENTED_EDGE('',*,*,#1135,.F.);
#1517=ORIENTED_EDGE('',*,*,#1126,.F.);
#1518=ORIENTED_EDGE('',*,*,#1136,.F.);
#1519=ORIENTED_EDGE('',*,*,#1133,.F.);
#1520=ORIENTED_EDGE('',*,*,#1137,.F.);
#1521=ORIENTED_EDGE('',*,*,#1123,.F.);
#1522=ORIENTED_EDGE('',*,*,#1138,.F.);
#1523=ORIENTED_EDGE('',*,*,#1131,.F.);
#1524=ORIENTED_EDGE('',*,*,#1139,.T.);
#1525=ORIENTED_EDGE('',*,*,#1140,.F.);
#1526=ORIENTED_EDGE('',*,*,#1132,.F.);
#1527=ORIENTED_EDGE('',*,*,#1140,.T.);
#1528=ORIENTED_EDGE('',*,*,#1141,.F.);
#1529=ORIENTED_EDGE('',*,*,#1134,.T.);
#1530=ORIENTED_EDGE('',*,*,#1136,.T.);
#1531=ORIENTED_EDGE('',*,*,#1127,.F.);
#1532=ORIENTED_EDGE('',*,*,#1135,.T.);
#1533=ORIENTED_EDGE('',*,*,#1141,.T.);
#1534=ORIENTED_EDGE('',*,*,#1142,.T.);
#1535=ORIENTED_EDGE('',*,*,#1129,.T.);
#1536=ORIENTED_EDGE('',*,*,#1143,.F.);
#1537=ORIENTED_EDGE('',*,*,#1128,.T.);
#1538=ORIENTED_EDGE('',*,*,#1143,.T.);
#1539=ORIENTED_EDGE('',*,*,#1139,.F.);
#1540=ORIENTED_EDGE('',*,*,#1130,.F.);
#1541=ORIENTED_EDGE('',*,*,#1142,.F.);
#1542=ORIENTED_EDGE('',*,*,#1124,.F.);
#1543=ORIENTED_EDGE('',*,*,#1137,.T.);
#1544=ORIENTED_EDGE('',*,*,#1144,.F.);
#1545=ORIENTED_EDGE('',*,*,#1122,.F.);
#1546=ORIENTED_EDGE('',*,*,#1118,.F.);
#1547=ORIENTED_EDGE('',*,*,#1125,.T.);
#1548=ORIENTED_EDGE('',*,*,#1144,.T.);
#1549=ORIENTED_EDGE('',*,*,#1138,.T.);
#1550=ORIENTED_EDGE('',*,*,#1121,.T.);
#1551=ORIENTED_EDGE('',*,*,#1145,.F.);
#1552=ORIENTED_EDGE('',*,*,#1146,.T.);
#1553=ORIENTED_EDGE('',*,*,#1147,.T.);
#1554=ORIENTED_EDGE('',*,*,#1146,.F.);
#1555=ORIENTED_EDGE('',*,*,#1148,.T.);
#1556=ORIENTED_EDGE('',*,*,#1149,.F.);
#1557=ORIENTED_EDGE('',*,*,#1150,.F.);
#1558=ORIENTED_EDGE('',*,*,#1151,.T.);
#1559=ORIENTED_EDGE('',*,*,#1152,.T.);
#1560=ORIENTED_EDGE('',*,*,#1153,.F.);
#1561=ORIENTED_EDGE('',*,*,#1154,.F.);
#1562=ORIENTED_EDGE('',*,*,#1149,.T.);
#1563=ORIENTED_EDGE('',*,*,#1155,.T.);
#1564=ORIENTED_EDGE('',*,*,#1156,.F.);
#1565=ORIENTED_EDGE('',*,*,#1157,.F.);
#1566=ORIENTED_EDGE('',*,*,#1153,.T.);
#1567=ORIENTED_EDGE('',*,*,#1158,.T.);
#1568=ORIENTED_EDGE('',*,*,#1159,.F.);
#1569=ORIENTED_EDGE('',*,*,#1160,.F.);
#1570=ORIENTED_EDGE('',*,*,#1156,.T.);
#1571=ORIENTED_EDGE('',*,*,#1161,.T.);
#1572=ORIENTED_EDGE('',*,*,#1151,.F.);
#1573=ORIENTED_EDGE('',*,*,#1162,.F.);
#1574=ORIENTED_EDGE('',*,*,#1159,.T.);
#1575=ORIENTED_EDGE('',*,*,#1150,.T.);
#1576=ORIENTED_EDGE('',*,*,#1154,.T.);
#1577=ORIENTED_EDGE('',*,*,#1157,.T.);
#1578=ORIENTED_EDGE('',*,*,#1160,.T.);
#1579=ORIENTED_EDGE('',*,*,#1162,.T.);
#1580=ORIENTED_EDGE('',*,*,#1147,.F.);
#1581=ORIENTED_EDGE('',*,*,#1148,.F.);
#1582=ORIENTED_EDGE('',*,*,#1161,.F.);
#1583=ORIENTED_EDGE('',*,*,#1158,.F.);
#1584=ORIENTED_EDGE('',*,*,#1155,.F.);
#1585=ORIENTED_EDGE('',*,*,#1152,.F.);
#1586=ORIENTED_EDGE('',*,*,#1145,.T.);
#1587=ORIENTED_EDGE('',*,*,#1163,.F.);
#1588=ORIENTED_EDGE('',*,*,#1164,.F.);
#1589=ORIENTED_EDGE('',*,*,#1165,.T.);
#1590=ORIENTED_EDGE('',*,*,#1166,.F.);
#1591=ORIENTED_EDGE('',*,*,#1165,.F.);
#1592=ORIENTED_EDGE('',*,*,#1167,.F.);
#1593=ORIENTED_EDGE('',*,*,#1168,.F.);
#1594=ORIENTED_EDGE('',*,*,#1169,.T.);
#1595=ORIENTED_EDGE('',*,*,#1170,.F.);
#1596=ORIENTED_EDGE('',*,*,#1169,.F.);
#1597=ORIENTED_EDGE('',*,*,#1167,.T.);
#1598=ORIENTED_EDGE('',*,*,#1168,.T.);
#1599=ORIENTED_EDGE('',*,*,#1171,.T.);
#1600=ORIENTED_EDGE('',*,*,#1172,.F.);
#1601=ORIENTED_EDGE('',*,*,#1171,.F.);
#1602=ORIENTED_EDGE('',*,*,#1163,.T.);
#1603=ORIENTED_EDGE('',*,*,#1164,.T.);
#1604=ORIENTED_EDGE('',*,*,#1173,.T.);
#1605=ORIENTED_EDGE('',*,*,#1174,.F.);
#1606=ORIENTED_EDGE('',*,*,#1173,.F.);
#1607=ORIENTED_EDGE('',*,*,#1175,.T.);
#1608=ORIENTED_EDGE('',*,*,#1176,.T.);
#1609=ORIENTED_EDGE('',*,*,#1177,.T.);
#1610=ORIENTED_EDGE('',*,*,#1178,.T.);
#1611=ORIENTED_EDGE('',*,*,#1166,.T.);
#1612=ORIENTED_EDGE('',*,*,#1170,.T.);
#1613=ORIENTED_EDGE('',*,*,#1179,.F.);
#1614=ORIENTED_EDGE('',*,*,#1180,.F.);
#1615=ORIENTED_EDGE('',*,*,#1181,.F.);
#1616=ORIENTED_EDGE('',*,*,#1182,.F.);
#1617=ORIENTED_EDGE('',*,*,#1174,.T.);
#1618=ORIENTED_EDGE('',*,*,#1172,.T.);
#1619=ORIENTED_EDGE('',*,*,#1183,.F.);
#1620=ORIENTED_EDGE('',*,*,#1184,.T.);
#1621=ORIENTED_EDGE('',*,*,#1185,.T.);
#1622=ORIENTED_EDGE('',*,*,#1179,.T.);
#1623=ORIENTED_EDGE('',*,*,#1186,.F.);
#1624=ORIENTED_EDGE('',*,*,#1187,.T.);
#1625=ORIENTED_EDGE('',*,*,#1183,.T.);
#1626=ORIENTED_EDGE('',*,*,#1182,.T.);
#1627=ORIENTED_EDGE('',*,*,#1188,.F.);
#1628=ORIENTED_EDGE('',*,*,#1189,.T.);
#1629=ORIENTED_EDGE('',*,*,#1186,.T.);
#1630=ORIENTED_EDGE('',*,*,#1181,.T.);
#1631=ORIENTED_EDGE('',*,*,#1185,.F.);
#1632=ORIENTED_EDGE('',*,*,#1190,.T.);
#1633=ORIENTED_EDGE('',*,*,#1188,.T.);
#1634=ORIENTED_EDGE('',*,*,#1180,.T.);
#1635=ORIENTED_EDGE('',*,*,#1191,.F.);
#1636=ORIENTED_EDGE('',*,*,#1187,.F.);
#1637=ORIENTED_EDGE('',*,*,#1192,.F.);
#1638=ORIENTED_EDGE('',*,*,#1178,.F.);
#1639=ORIENTED_EDGE('',*,*,#1192,.T.);
#1640=ORIENTED_EDGE('',*,*,#1189,.F.);
#1641=ORIENTED_EDGE('',*,*,#1193,.F.);
#1642=ORIENTED_EDGE('',*,*,#1175,.F.);
#1643=ORIENTED_EDGE('',*,*,#1191,.T.);
#1644=ORIENTED_EDGE('',*,*,#1177,.F.);
#1645=ORIENTED_EDGE('',*,*,#1194,.F.);
#1646=ORIENTED_EDGE('',*,*,#1184,.F.);
#1647=ORIENTED_EDGE('',*,*,#1193,.T.);
#1648=ORIENTED_EDGE('',*,*,#1190,.F.);
#1649=ORIENTED_EDGE('',*,*,#1194,.T.);
#1650=ORIENTED_EDGE('',*,*,#1176,.F.);
#1651=ORIENTED_EDGE('',*,*,#1195,.F.);
#1652=ORIENTED_EDGE('',*,*,#1196,.T.);
#1653=ORIENTED_EDGE('',*,*,#1197,.F.);
#1654=ORIENTED_EDGE('',*,*,#1196,.F.);
#1655=ORIENTED_EDGE('',*,*,#1198,.F.);
#1656=ORIENTED_EDGE('',*,*,#1199,.T.);
#1657=ORIENTED_EDGE('',*,*,#1200,.F.);
#1658=ORIENTED_EDGE('',*,*,#1199,.F.);
#1659=ORIENTED_EDGE('',*,*,#1201,.T.);
#1660=ORIENTED_EDGE('',*,*,#1202,.T.);
#1661=ORIENTED_EDGE('',*,*,#1203,.F.);
#1662=ORIENTED_EDGE('',*,*,#1202,.F.);
#1663=ORIENTED_EDGE('',*,*,#1197,.T.);
#1664=ORIENTED_EDGE('',*,*,#1204,.T.);
#1665=ORIENTED_EDGE('',*,*,#1198,.T.);
#1666=ORIENTED_EDGE('',*,*,#1204,.F.);
#1667=ORIENTED_EDGE('',*,*,#1200,.T.);
#1668=ORIENTED_EDGE('',*,*,#1195,.T.);
#1669=ORIENTED_EDGE('',*,*,#1201,.F.);
#1670=ORIENTED_EDGE('',*,*,#1203,.T.);
#1671=ORIENTED_EDGE('',*,*,#1205,.T.);
#1672=ORIENTED_EDGE('',*,*,#1206,.T.);
#1673=ORIENTED_EDGE('',*,*,#1207,.F.);
#1674=ORIENTED_EDGE('',*,*,#1206,.F.);
#1675=ORIENTED_EDGE('',*,*,#1208,.T.);
#1676=ORIENTED_EDGE('',*,*,#1209,.T.);
#1677=ORIENTED_EDGE('',*,*,#1210,.F.);
#1678=ORIENTED_EDGE('',*,*,#1209,.F.);
#1679=ORIENTED_EDGE('',*,*,#1211,.T.);
#1680=ORIENTED_EDGE('',*,*,#1212,.T.);
#1681=ORIENTED_EDGE('',*,*,#1213,.T.);
#1682=ORIENTED_EDGE('',*,*,#1214,.T.);
#1683=ORIENTED_EDGE('',*,*,#1205,.F.);
#1684=ORIENTED_EDGE('',*,*,#1208,.F.);
#1685=ORIENTED_EDGE('',*,*,#1215,.F.);
#1686=ORIENTED_EDGE('',*,*,#1216,.F.);
#1687=ORIENTED_EDGE('',*,*,#1217,.F.);
#1688=ORIENTED_EDGE('',*,*,#1218,.F.);
#1689=ORIENTED_EDGE('',*,*,#1210,.T.);
#1690=ORIENTED_EDGE('',*,*,#1207,.T.);
#1691=ORIENTED_EDGE('',*,*,#1215,.T.);
#1692=ORIENTED_EDGE('',*,*,#1219,.F.);
#1693=ORIENTED_EDGE('',*,*,#1211,.F.);
#1694=ORIENTED_EDGE('',*,*,#1220,.T.);
#1695=ORIENTED_EDGE('',*,*,#1218,.T.);
#1696=ORIENTED_EDGE('',*,*,#1221,.F.);
#1697=ORIENTED_EDGE('',*,*,#1212,.F.);
#1698=ORIENTED_EDGE('',*,*,#1219,.T.);
#1699=ORIENTED_EDGE('',*,*,#1217,.T.);
#1700=ORIENTED_EDGE('',*,*,#1222,.F.);
#1701=ORIENTED_EDGE('',*,*,#1213,.F.);
#1702=ORIENTED_EDGE('',*,*,#1221,.T.);
#1703=ORIENTED_EDGE('',*,*,#1216,.T.);
#1704=ORIENTED_EDGE('',*,*,#1220,.F.);
#1705=ORIENTED_EDGE('',*,*,#1214,.F.);
#1706=ORIENTED_EDGE('',*,*,#1222,.T.);
#1707=TOROIDAL_SURFACE('',#1963,2.5,0.5);
#1708=TOROIDAL_SURFACE('',#1968,2.5,0.5);
#1709=TOROIDAL_SURFACE('',#1992,11.7723008899906,0.5);
#1710=TOROIDAL_SURFACE('',#1994,11.7723008899906,0.5);
#1711=TOROIDAL_SURFACE('',#2050,1.99999999999999,0.25);
#1712=TOROIDAL_SURFACE('',#2081,2.5,0.5);
#1713=TOROIDAL_SURFACE('',#2086,2.5,0.5);
#1714=TOROIDAL_SURFACE('',#2110,11.7723008899906,0.5);
#1715=TOROIDAL_SURFACE('',#2112,11.7723008899906,0.5);
#1716=TOROIDAL_SURFACE('',#2116,3.5,0.5);
#1717=TOROIDAL_SURFACE('',#2120,3.5,0.5);
#1718=ADVANCED_FACE('',(#490),#1707,.T.);
#1719=ADVANCED_FACE('',(#491),#1708,.T.);
#1720=ADVANCED_FACE('',(#492),#464,.F.);
#1721=ADVANCED_FACE('',(#493),#465,.F.);
#1722=ADVANCED_FACE('',(#494,#205,#206),#232,.T.);
#1723=ADVANCED_FACE('',(#495,#207,#208),#233,.F.);
#1724=ADVANCED_FACE('',(#496),#466,.T.);
#1725=ADVANCED_FACE('',(#497),#234,.F.);
#1726=ADVANCED_FACE('',(#498),#467,.T.);
#1727=ADVANCED_FACE('',(#499),#235,.F.);
#1728=ADVANCED_FACE('',(#500),#468,.T.);
#1729=ADVANCED_FACE('',(#501),#1709,.T.);
#1730=ADVANCED_FACE('',(#502),#1710,.T.);
#1731=ADVANCED_FACE('',(#503),#469,.T.);
#1732=ADVANCED_FACE('',(#504),#470,.F.);
#1733=ADVANCED_FACE('',(#505),#138,.F.);
#1734=ADVANCED_FACE('',(#506),#139,.F.);
#1735=ADVANCED_FACE('',(#507),#140,.F.);
#1736=ADVANCED_FACE('',(#508,#209),#236,.F.);
#1737=ADVANCED_FACE('',(#509,#210),#237,.T.);
#1738=ADVANCED_FACE('',(#510),#238,.F.);
#1739=ADVANCED_FACE('',(#511),#239,.F.);
#1740=ADVANCED_FACE('',(#512),#141,.T.);
#1741=ADVANCED_FACE('',(#513),#471,.F.);
#1742=ADVANCED_FACE('',(#514),#142,.F.);
#1743=ADVANCED_FACE('',(#515),#143,.F.);
#1744=ADVANCED_FACE('',(#516),#144,.F.);
#1745=ADVANCED_FACE('',(#517),#145,.F.);
#1746=ADVANCED_FACE('',(#518,#211),#240,.F.);
#1747=ADVANCED_FACE('',(#519,#212),#241,.T.);
#1748=ADVANCED_FACE('',(#520),#242,.F.);
#1749=ADVANCED_FACE('',(#521),#243,.F.);
#1750=ADVANCED_FACE('',(#522),#146,.T.);
#1751=ADVANCED_FACE('',(#523),#472,.F.);
#1752=ADVANCED_FACE('',(#524),#147,.F.);
#1753=ADVANCED_FACE('',(#525),#148,.F.);
#1754=ADVANCED_FACE('',(#526),#149,.F.);
#1755=ADVANCED_FACE('',(#527),#150,.F.);
#1756=ADVANCED_FACE('',(#528),#244,.F.);
#1757=ADVANCED_FACE('',(#529,#213),#245,.F.);
#1758=ADVANCED_FACE('',(#530,#214),#246,.T.);
#1759=ADVANCED_FACE('',(#531),#247,.F.);
#1760=ADVANCED_FACE('',(#532),#151,.T.);
#1761=ADVANCED_FACE('',(#533),#473,.F.);
#1762=ADVANCED_FACE('',(#534),#474,.F.);
#1763=ADVANCED_FACE('',(#535),#152,.F.);
#1764=ADVANCED_FACE('',(#536),#153,.F.);
#1765=ADVANCED_FACE('',(#537),#154,.F.);
#1766=ADVANCED_FACE('',(#538),#248,.F.);
#1767=ADVANCED_FACE('',(#539,#215,#216),#249,.T.);
#1768=ADVANCED_FACE('',(#540,#217,#218),#250,.F.);
#1769=ADVANCED_FACE('',(#541),#251,.F.);
#1770=ADVANCED_FACE('',(#542),#252,.F.);
#1771=ADVANCED_FACE('',(#543),#253,.T.);
#1772=ADVANCED_FACE('',(#544),#155,.T.);
#1773=ADVANCED_FACE('',(#545),#475,.T.);
#1774=ADVANCED_FACE('',(#546),#476,.T.);
#1775=ADVANCED_FACE('',(#547,#219),#254,.T.);
#1776=ADVANCED_FACE('',(#548),#255,.F.);
#1777=ADVANCED_FACE('',(#549),#256,.T.);
#1778=ADVANCED_FACE('',(#550),#1711,.T.);
#1779=ADVANCED_FACE('',(#551),#15,.F.);
#1780=ADVANCED_FACE('',(#552),#16,.T.);
#1781=ADVANCED_FACE('',(#553),#17,.T.);
#1782=ADVANCED_FACE('',(#554,#220),#257,.F.);
#1783=ADVANCED_FACE('',(#555),#258,.T.);
#1784=ADVANCED_FACE('',(#556),#18,.T.);
#1785=ADVANCED_FACE('',(#557),#19,.T.);
#1786=ADVANCED_FACE('',(#558),#259,.T.);
#1787=ADVANCED_FACE('',(#559),#260,.F.);
#1788=ADVANCED_FACE('',(#560),#261,.F.);
#1789=ADVANCED_FACE('',(#561),#20,.F.);
#1790=ADVANCED_FACE('',(#562),#262,.T.);
#1791=ADVANCED_FACE('',(#563),#477,.F.);
#1792=ADVANCED_FACE('',(#564),#156,.F.);
#1793=ADVANCED_FACE('',(#565),#157,.F.);
#1794=ADVANCED_FACE('',(#566),#158,.F.);
#1795=ADVANCED_FACE('',(#567),#159,.F.);
#1796=ADVANCED_FACE('',(#568),#160,.F.);
#1797=ADVANCED_FACE('',(#569,#221),#263,.T.);
#1798=ADVANCED_FACE('',(#570,#222),#264,.F.);
#1799=ADVANCED_FACE('',(#571),#1712,.T.);
#1800=ADVANCED_FACE('',(#572),#1713,.T.);
#1801=ADVANCED_FACE('',(#573),#478,.F.);
#1802=ADVANCED_FACE('',(#574),#479,.F.);
#1803=ADVANCED_FACE('',(#575,#223,#224),#265,.T.);
#1804=ADVANCED_FACE('',(#576,#225,#226),#266,.F.);
#1805=ADVANCED_FACE('',(#577),#480,.T.);
#1806=ADVANCED_FACE('',(#578),#267,.F.);
#1807=ADVANCED_FACE('',(#579),#481,.T.);
#1808=ADVANCED_FACE('',(#580),#268,.F.);
#1809=ADVANCED_FACE('',(#581),#482,.T.);
#1810=ADVANCED_FACE('',(#582),#1714,.T.);
#1811=ADVANCED_FACE('',(#583),#1715,.T.);
#1812=ADVANCED_FACE('',(#584),#483,.T.);
#1813=ADVANCED_FACE('',(#585),#1716,.T.);
#1814=ADVANCED_FACE('',(#586),#1717,.T.);
#1815=ADVANCED_FACE('',(#587),#484,.T.);
#1816=ADVANCED_FACE('',(#588),#485,.T.);
#1817=ADVANCED_FACE('',(#589),#269,.F.);
#1818=ADVANCED_FACE('',(#590,#227),#270,.T.);
#1819=ADVANCED_FACE('',(#591),#271,.T.);
#1820=ADVANCED_FACE('',(#592),#486,.F.);
#1821=ADVANCED_FACE('',(#593),#487,.F.);
#1822=ADVANCED_FACE('',(#594,#228,#229),#272,.T.);
#1823=ADVANCED_FACE('',(#595,#230,#231),#273,.F.);
#1824=ADVANCED_FACE('',(#596),#488,.T.);
#1825=ADVANCED_FACE('',(#597),#274,.F.);
#1826=ADVANCED_FACE('',(#598),#489,.T.);
#1827=ADVANCED_FACE('',(#599),#275,.F.);
#1828=CLOSED_SHELL('',(#1718,#1719,#1720,#1721,#1722,#1723,#1724,#1725,
#1726,#1727,#1728,#1729,#1730,#1731));
#1829=CLOSED_SHELL('',(#1732,#1733,#1734,#1735,#1736,#1737,#1738,#1739,
#1740));
#1830=CLOSED_SHELL('',(#1741,#1742,#1743,#1744,#1745,#1746,#1747,#1748,
#1749,#1750));
#1831=CLOSED_SHELL('',(#1751,#1752,#1753,#1754,#1755,#1756,#1757,#1758,
#1759,#1760));
#1832=CLOSED_SHELL('',(#1761,#1762,#1763,#1764,#1765,#1766,#1767,#1768,
#1769,#1770,#1771,#1772));
#1833=CLOSED_SHELL('',(#1773,#1774,#1775,#1776,#1777));
#1834=CLOSED_SHELL('',(#1778,#1779,#1780,#1781,#1782,#1783,#1784,#1785,
#1786,#1787,#1788,#1789,#1790));
#1835=CLOSED_SHELL('',(#1791,#1792,#1793,#1794,#1795,#1796,#1797,#1798));
#1836=CLOSED_SHELL('',(#1799,#1800,#1801,#1802,#1803,#1804,#1805,#1806,
#1807,#1808,#1809,#1810,#1811,#1812));
#1837=CLOSED_SHELL('',(#1813,#1814,#1815,#1816,#1817,#1818,#1819));
#1838=CLOSED_SHELL('',(#1820,#1821,#1822,#1823,#1824,#1825,#1826,#1827));
#1839=DERIVED_UNIT_ELEMENT(#1861,1.);
#1840=DERIVED_UNIT_ELEMENT(#12139,-3.);
#1841=DERIVED_UNIT_ELEMENT(#1861,1.);
#1842=DERIVED_UNIT_ELEMENT(#12139,-3.);
#1843=DERIVED_UNIT_ELEMENT(#1861,1.);
#1844=DERIVED_UNIT_ELEMENT(#12139,-3.);
#1845=DERIVED_UNIT_ELEMENT(#1861,1.);
#1846=DERIVED_UNIT_ELEMENT(#12139,-3.);
#1847=DERIVED_UNIT_ELEMENT(#1861,1.);
#1848=DERIVED_UNIT_ELEMENT(#12139,-3.);
#1849=DERIVED_UNIT_ELEMENT(#1861,1.);
#1850=DERIVED_UNIT_ELEMENT(#12139,-3.);
#1851=DERIVED_UNIT_ELEMENT(#1861,1.);
#1852=DERIVED_UNIT_ELEMENT(#12139,-3.);
#1853=DERIVED_UNIT_ELEMENT(#1861,1.);
#1854=DERIVED_UNIT_ELEMENT(#12139,-3.);
#1855=DERIVED_UNIT_ELEMENT(#1861,1.);
#1856=DERIVED_UNIT_ELEMENT(#12139,-3.);
#1857=DERIVED_UNIT_ELEMENT(#1861,1.);
#1858=DERIVED_UNIT_ELEMENT(#12139,-3.);
#1859=DERIVED_UNIT_ELEMENT(#1861,1.);
#1860=DERIVED_UNIT_ELEMENT(#12139,-3.);
#1861=(
MASS_UNIT()
NAMED_UNIT(*)
SI_UNIT(.KILO.,.GRAM.)
);
#1862=DERIVED_UNIT((#1839,#1840));
#1863=DERIVED_UNIT((#1841,#1842));
#1864=DERIVED_UNIT((#1843,#1844));
#1865=DERIVED_UNIT((#1845,#1846));
#1866=DERIVED_UNIT((#1847,#1848));
#1867=DERIVED_UNIT((#1849,#1850));
#1868=DERIVED_UNIT((#1851,#1852));
#1869=DERIVED_UNIT((#1853,#1854));
#1870=DERIVED_UNIT((#1855,#1856));
#1871=DERIVED_UNIT((#1857,#1858));
#1872=DERIVED_UNIT((#1859,#1860));
#1873=MEASURE_REPRESENTATION_ITEM('density measure',
POSITIVE_RATIO_MEASURE(7850.),#1862);
#1874=MEASURE_REPRESENTATION_ITEM('density measure',
POSITIVE_RATIO_MEASURE(7850.),#1863);
#1875=MEASURE_REPRESENTATION_ITEM('density measure',
POSITIVE_RATIO_MEASURE(7850.),#1864);
#1876=MEASURE_REPRESENTATION_ITEM('density measure',
POSITIVE_RATIO_MEASURE(7850.),#1865);
#1877=MEASURE_REPRESENTATION_ITEM('density measure',
POSITIVE_RATIO_MEASURE(7850.),#1866);
#1878=MEASURE_REPRESENTATION_ITEM('density measure',
POSITIVE_RATIO_MEASURE(7850.),#1867);
#1879=MEASURE_REPRESENTATION_ITEM('density measure',
POSITIVE_RATIO_MEASURE(7850.),#1868);
#1880=MEASURE_REPRESENTATION_ITEM('density measure',
POSITIVE_RATIO_MEASURE(7850.),#1869);
#1881=MEASURE_REPRESENTATION_ITEM('density measure',
POSITIVE_RATIO_MEASURE(7850.),#1870);
#1882=MEASURE_REPRESENTATION_ITEM('density measure',
POSITIVE_RATIO_MEASURE(7850.),#1871);
#1883=MEASURE_REPRESENTATION_ITEM('density measure',
POSITIVE_RATIO_MEASURE(7850.),#1872);
#1884=PROPERTY_DEFINITION_REPRESENTATION(#1939,#1906);
#1885=PROPERTY_DEFINITION_REPRESENTATION(#1940,#1907);
#1886=PROPERTY_DEFINITION_REPRESENTATION(#1941,#1908);
#1887=PROPERTY_DEFINITION_REPRESENTATION(#1942,#1909);
#1888=PROPERTY_DEFINITION_REPRESENTATION(#1943,#1910);
#1889=PROPERTY_DEFINITION_REPRESENTATION(#1944,#1911);
#1890=PROPERTY_DEFINITION_REPRESENTATION(#1945,#1912);
#1891=PROPERTY_DEFINITION_REPRESENTATION(#1946,#1913);
#1892=PROPERTY_DEFINITION_REPRESENTATION(#1947,#1914);
#1893=PROPERTY_DEFINITION_REPRESENTATION(#1948,#1915);
#1894=PROPERTY_DEFINITION_REPRESENTATION(#1949,#1916);
#1895=PROPERTY_DEFINITION_REPRESENTATION(#1950,#1917);
#1896=PROPERTY_DEFINITION_REPRESENTATION(#1951,#1918);
#1897=PROPERTY_DEFINITION_REPRESENTATION(#1952,#1919);
#1898=PROPERTY_DEFINITION_REPRESENTATION(#1953,#1920);
#1899=PROPERTY_DEFINITION_REPRESENTATION(#1954,#1921);
#1900=PROPERTY_DEFINITION_REPRESENTATION(#1955,#1922);
#1901=PROPERTY_DEFINITION_REPRESENTATION(#1956,#1923);
#1902=PROPERTY_DEFINITION_REPRESENTATION(#1957,#1924);
#1903=PROPERTY_DEFINITION_REPRESENTATION(#1958,#1925);
#1904=PROPERTY_DEFINITION_REPRESENTATION(#1959,#1926);
#1905=PROPERTY_DEFINITION_REPRESENTATION(#1960,#1927);
#1906=REPRESENTATION('material name',(#1928),#12125);
#1907=REPRESENTATION('density',(#1873),#12125);
#1908=REPRESENTATION('material name',(#1929),#12126);
#1909=REPRESENTATION('density',(#1874),#12126);
#1910=REPRESENTATION('material name',(#1930),#12127);
#1911=REPRESENTATION('density',(#1875),#12127);
#1912=REPRESENTATION('material name',(#1931),#12129);
#1913=REPRESENTATION('density',(#1876),#12129);
#1914=REPRESENTATION('material name',(#1932),#12130);
#1915=REPRESENTATION('density',(#1877),#12130);
#1916=REPRESENTATION('material name',(#1933),#12131);
#1917=REPRESENTATION('density',(#1878),#12131);
#1918=REPRESENTATION('material name',(#1934),#12132);
#1919=REPRESENTATION('density',(#1879),#12132);
#1920=REPRESENTATION('material name',(#1935),#12133);
#1921=REPRESENTATION('density',(#1880),#12133);
#1922=REPRESENTATION('material name',(#1936),#12134);
#1923=REPRESENTATION('density',(#1881),#12134);
#1924=REPRESENTATION('material name',(#1937),#12135);
#1925=REPRESENTATION('density',(#1882),#12135);
#1926=REPRESENTATION('material name',(#1938),#12136);
#1927=REPRESENTATION('density',(#1883),#12136);
#1928=DESCRIPTIVE_REPRESENTATION_ITEM('Steel','Steel');
#1929=DESCRIPTIVE_REPRESENTATION_ITEM('Steel','Steel');
#1930=DESCRIPTIVE_REPRESENTATION_ITEM('Steel','Steel');
#1931=DESCRIPTIVE_REPRESENTATION_ITEM('Steel','Steel');
#1932=DESCRIPTIVE_REPRESENTATION_ITEM('Steel','Steel');
#1933=DESCRIPTIVE_REPRESENTATION_ITEM('Steel','Steel');
#1934=DESCRIPTIVE_REPRESENTATION_ITEM('Steel','Steel');
#1935=DESCRIPTIVE_REPRESENTATION_ITEM('Steel','Steel');
#1936=DESCRIPTIVE_REPRESENTATION_ITEM('Steel','Steel');
#1937=DESCRIPTIVE_REPRESENTATION_ITEM('Steel','Steel');
#1938=DESCRIPTIVE_REPRESENTATION_ITEM('Steel','Steel');
#1939=PROPERTY_DEFINITION('material property','material name',#12198);
#1940=PROPERTY_DEFINITION('material property','density of part',#12198);
#1941=PROPERTY_DEFINITION('material property','material name',#12199);
#1942=PROPERTY_DEFINITION('material property','density of part',#12199);
#1943=PROPERTY_DEFINITION('material property','material name',#12200);
#1944=PROPERTY_DEFINITION('material property','density of part',#12200);
#1945=PROPERTY_DEFINITION('material property','material name',#12202);
#1946=PROPERTY_DEFINITION('material property','density of part',#12202);
#1947=PROPERTY_DEFINITION('material property','material name',#12203);
#1948=PROPERTY_DEFINITION('material property','density of part',#12203);
#1949=PROPERTY_DEFINITION('material property','material name',#12204);
#1950=PROPERTY_DEFINITION('material property','density of part',#12204);
#1951=PROPERTY_DEFINITION('material property','material name',#12205);
#1952=PROPERTY_DEFINITION('material property','density of part',#12205);
#1953=PROPERTY_DEFINITION('material property','material name',#12206);
#1954=PROPERTY_DEFINITION('material property','density of part',#12206);
#1955=PROPERTY_DEFINITION('material property','material name',#12207);
#1956=PROPERTY_DEFINITION('material property','density of part',#12207);
#1957=PROPERTY_DEFINITION('material property','material name',#12208);
#1958=PROPERTY_DEFINITION('material property','density of part',#12208);
#1959=PROPERTY_DEFINITION('material property','material name',#12209);
#1960=PROPERTY_DEFINITION('material property','density of part',#12209);
#1961=AXIS2_PLACEMENT_3D('',#2652,#2160,#2161);
#1962=AXIS2_PLACEMENT_3D('',#2653,#2162,#2163);
#1963=AXIS2_PLACEMENT_3D('',#2654,#2164,#2165);
#1964=AXIS2_PLACEMENT_3D('',#2657,#2166,#2167);
#1965=AXIS2_PLACEMENT_3D('',#2658,#2168,#2169);
#1966=AXIS2_PLACEMENT_3D('',#2660,#2170,#2171);
#1967=AXIS2_PLACEMENT_3D('',#2661,#2172,#2173);
#1968=AXIS2_PLACEMENT_3D('',#2662,#2174,#2175);
#1969=AXIS2_PLACEMENT_3D('',#2665,#2176,#2177);
#1970=AXIS2_PLACEMENT_3D('',#2666,#2178,#2179);
#1971=AXIS2_PLACEMENT_3D('',#2668,#2180,#2181);
#1972=AXIS2_PLACEMENT_3D('',#2669,#2182,#2183);
#1973=AXIS2_PLACEMENT_3D('',#2670,#2184,#2185);
#1974=AXIS2_PLACEMENT_3D('',#2673,#2187,#2188);
#1975=AXIS2_PLACEMENT_3D('',#2674,#2189,#2190);
#1976=AXIS2_PLACEMENT_3D('',#2677,#2192,#2193);
#1977=AXIS2_PLACEMENT_3D('',#2678,#2194,#2195);
#1978=AXIS2_PLACEMENT_3D('',#2681,#2196,#2197);
#1979=AXIS2_PLACEMENT_3D('',#2685,#2199,#2200);
#1980=AXIS2_PLACEMENT_3D('',#2687,#2202,#2203);
#1981=AXIS2_PLACEMENT_3D('',#2690,#2204,#2205);
#1982=AXIS2_PLACEMENT_3D('',#2694,#2207,#2208);
#1983=AXIS2_PLACEMENT_3D('',#2696,#2210,#2211);
#1984=AXIS2_PLACEMENT_3D('',#2700,#2213,#2214);
#1985=AXIS2_PLACEMENT_3D('',#2702,#2216,#2217);
#1986=AXIS2_PLACEMENT_3D('',#2706,#2220,#2221);
#1987=AXIS2_PLACEMENT_3D('',#2709,#2223,#2224);
#1988=AXIS2_PLACEMENT_3D('',#2710,#2225,#2226);
#1989=AXIS2_PLACEMENT_3D('',#2712,#2228,#2229);
#1990=AXIS2_PLACEMENT_3D('',#2713,#2230,#2231);
#1991=AXIS2_PLACEMENT_3D('',#2714,#2232,#2233);
#1992=AXIS2_PLACEMENT_3D('',#2715,#2234,#2235);
#1993=AXIS2_PLACEMENT_3D('',#2716,#2236,#2237);
#1994=AXIS2_PLACEMENT_3D('',#2717,#2238,#2239);
#1995=AXIS2_PLACEMENT_3D('',#2718,#2240,#2241);
#1996=AXIS2_PLACEMENT_3D('',#2719,#2242,#2243);
#1997=AXIS2_PLACEMENT_3D('',#2720,#2244,#2245);
#1998=AXIS2_PLACEMENT_3D('',#2721,#2246,#2247);
#1999=AXIS2_PLACEMENT_3D('',#2723,#2248,#2249);
#2000=AXIS2_PLACEMENT_3D('',#2726,#2251,#2252);
#2001=AXIS2_PLACEMENT_3D('',#2845,#2256,#2257);
#2002=AXIS2_PLACEMENT_3D('',#3181,#2260,#2261);
#2003=AXIS2_PLACEMENT_3D('',#3297,#2264,#2265);
#2004=AXIS2_PLACEMENT_3D('',#3305,#2267,#2268);
#2005=AXIS2_PLACEMENT_3D('',#3618,#2269,#2270);
#2006=AXIS2_PLACEMENT_3D('',#3619,#2271,#2272);
#2007=AXIS2_PLACEMENT_3D('',#3621,#2273,#2274);
#2008=AXIS2_PLACEMENT_3D('',#3624,#2276,#2277);
#2009=AXIS2_PLACEMENT_3D('',#3910,#2283,#2284);
#2010=AXIS2_PLACEMENT_3D('',#4296,#2285,#2286);
#2011=AXIS2_PLACEMENT_3D('',#4300,#2289,#2290);
#2012=AXIS2_PLACEMENT_3D('',#4304,#2293,#2294);
#2013=AXIS2_PLACEMENT_3D('',#4592,#2295,#2296);
#2014=AXIS2_PLACEMENT_3D('',#4593,#2297,#2298);
#2015=AXIS2_PLACEMENT_3D('',#4594,#2299,#2300);
#2016=AXIS2_PLACEMENT_3D('',#4596,#2301,#2302);
#2017=AXIS2_PLACEMENT_3D('',#4599,#2304,#2305);
#2018=AXIS2_PLACEMENT_3D('',#4779,#2312,#2313);
#2019=AXIS2_PLACEMENT_3D('',#4789,#2316,#2317);
#2020=AXIS2_PLACEMENT_3D('',#4791,#2319,#2320);
#2021=AXIS2_PLACEMENT_3D('',#4860,#2322,#2323);
#2022=AXIS2_PLACEMENT_3D('',#5021,#2324,#2325);
#2023=AXIS2_PLACEMENT_3D('',#5022,#2326,#2327);
#2024=AXIS2_PLACEMENT_3D('',#5024,#2328,#2329);
#2025=AXIS2_PLACEMENT_3D('',#5027,#2331,#2332);
#2026=AXIS2_PLACEMENT_3D('',#5028,#2333,#2334);
#2027=AXIS2_PLACEMENT_3D('',#5030,#2335,#2336);
#2028=AXIS2_PLACEMENT_3D('',#5033,#2338,#2339);
#2029=AXIS2_PLACEMENT_3D('',#5098,#2343,#2344);
#2030=AXIS2_PLACEMENT_3D('',#5165,#2347,#2348);
#2031=AXIS2_PLACEMENT_3D('',#5168,#2351,#2352);
#2032=AXIS2_PLACEMENT_3D('',#5174,#2356,#2357);
#2033=AXIS2_PLACEMENT_3D('',#5187,#2361,#2362);
#2034=AXIS2_PLACEMENT_3D('',#5190,#2365,#2366);
#2035=AXIS2_PLACEMENT_3D('',#5192,#2368,#2369);
#2036=AXIS2_PLACEMENT_3D('',#5253,#2370,#2371);
#2037=AXIS2_PLACEMENT_3D('',#5254,#2372,#2373);
#2038=AXIS2_PLACEMENT_3D('',#5256,#2374,#2375);
#2039=AXIS2_PLACEMENT_3D('',#5259,#2377,#2378);
#2040=AXIS2_PLACEMENT_3D('',#5260,#2379,#2380);
#2041=AXIS2_PLACEMENT_3D('',#5262,#2381,#2382);
#2042=AXIS2_PLACEMENT_3D('',#5265,#2384,#2385);
#2043=AXIS2_PLACEMENT_3D('',#5266,#2386,#2387);
#2044=AXIS2_PLACEMENT_3D('',#5267,#2388,#2389);
#2045=AXIS2_PLACEMENT_3D('',#5268,#2390,#2391);
#2046=AXIS2_PLACEMENT_3D('',#5269,#2392,#2393);
#2047=AXIS2_PLACEMENT_3D('',#5270,#2394,#2395);
#2048=AXIS2_PLACEMENT_3D('',#5271,#2396,#2397);
#2049=AXIS2_PLACEMENT_3D('',#5272,#2398,#2399);
#2050=AXIS2_PLACEMENT_3D('',#5273,#2400,#2401);
#2051=AXIS2_PLACEMENT_3D('',#5276,#2402,#2403);
#2052=AXIS2_PLACEMENT_3D('',#5277,#2404,#2405);
#2053=AXIS2_PLACEMENT_3D('',#5279,#2406,#2407);
#2054=AXIS2_PLACEMENT_3D('',#5280,#2408,#2409);
#2055=AXIS2_PLACEMENT_3D('',#5379,#2410,#2411);
#2056=AXIS2_PLACEMENT_3D('',#5381,#2412,#2413);
#2057=AXIS2_PLACEMENT_3D('',#5748,#2414,#2415);
#2058=AXIS2_PLACEMENT_3D('',#5790,#2416,#2417);
#2059=AXIS2_PLACEMENT_3D('',#7722,#2418,#2419);
#2060=AXIS2_PLACEMENT_3D('',#7918,#2420,#2421);
#2061=AXIS2_PLACEMENT_3D('',#9934,#2422,#2423);
#2062=AXIS2_PLACEMENT_3D('',#9935,#2424,#2425);
#2063=AXIS2_PLACEMENT_3D('',#9936,#2426,#2427);
#2064=AXIS2_PLACEMENT_3D('',#9939,#2429,#2430);
#2065=AXIS2_PLACEMENT_3D('',#9940,#2431,#2432);
#2066=AXIS2_PLACEMENT_3D('',#9943,#2434,#2435);
#2067=AXIS2_PLACEMENT_3D('',#11587,#2436,#2437);
#2068=AXIS2_PLACEMENT_3D('',#11588,#2438,#2439);
#2069=AXIS2_PLACEMENT_3D('',#11589,#2440,#2441);
#2070=AXIS2_PLACEMENT_3D('',#11590,#2442,#2443);
#2071=AXIS2_PLACEMENT_3D('',#11591,#2444,#2445);
#2072=AXIS2_PLACEMENT_3D('',#11592,#2446,#2447);
#2073=AXIS2_PLACEMENT_3D('',#11677,#2448,#2449);
#2074=AXIS2_PLACEMENT_3D('',#11678,#2450,#2451);
#2075=AXIS2_PLACEMENT_3D('',#11679,#2452,#2453);
#2076=AXIS2_PLACEMENT_3D('',#11681,#2454,#2455);
#2077=AXIS2_PLACEMENT_3D('',#11684,#2457,#2458);
#2078=AXIS2_PLACEMENT_3D('',#11966,#2464,#2465);
#2079=AXIS2_PLACEMENT_3D('',#11967,#2466,#2467);
#2080=AXIS2_PLACEMENT_3D('',#11968,#2468,#2469);
#2081=AXIS2_PLACEMENT_3D('',#11969,#2470,#2471);
#2082=AXIS2_PLACEMENT_3D('',#11972,#2472,#2473);
#2083=AXIS2_PLACEMENT_3D('',#11973,#2474,#2475);
#2084=AXIS2_PLACEMENT_3D('',#11975,#2476,#2477);
#2085=AXIS2_PLACEMENT_3D('',#11976,#2478,#2479);
#2086=AXIS2_PLACEMENT_3D('',#11977,#2480,#2481);
#2087=AXIS2_PLACEMENT_3D('',#11980,#2482,#2483);
#2088=AXIS2_PLACEMENT_3D('',#11981,#2484,#2485);
#2089=AXIS2_PLACEMENT_3D('',#11983,#2486,#2487);
#2090=AXIS2_PLACEMENT_3D('',#11984,#2488,#2489);
#2091=AXIS2_PLACEMENT_3D('',#11985,#2490,#2491);
#2092=AXIS2_PLACEMENT_3D('',#11988,#2493,#2494);
#2093=AXIS2_PLACEMENT_3D('',#11989,#2495,#2496);
#2094=AXIS2_PLACEMENT_3D('',#11992,#2498,#2499);
#2095=AXIS2_PLACEMENT_3D('',#11993,#2500,#2501);
#2096=AXIS2_PLACEMENT_3D('',#11996,#2502,#2503);
#2097=AXIS2_PLACEMENT_3D('',#12000,#2505,#2506);
#2098=AXIS2_PLACEMENT_3D('',#12002,#2508,#2509);
#2099=AXIS2_PLACEMENT_3D('',#12005,#2510,#2511);
#2100=AXIS2_PLACEMENT_3D('',#12009,#2513,#2514);
#2101=AXIS2_PLACEMENT_3D('',#12011,#2516,#2517);
#2102=AXIS2_PLACEMENT_3D('',#12015,#2519,#2520);
#2103=AXIS2_PLACEMENT_3D('',#12017,#2522,#2523);
#2104=AXIS2_PLACEMENT_3D('',#12021,#2526,#2527);
#2105=AXIS2_PLACEMENT_3D('',#12024,#2529,#2530);
#2106=AXIS2_PLACEMENT_3D('',#12025,#2531,#2532);
#2107=AXIS2_PLACEMENT_3D('',#12027,#2534,#2535);
#2108=AXIS2_PLACEMENT_3D('',#12028,#2536,#2537);
#2109=AXIS2_PLACEMENT_3D('',#12029,#2538,#2539);
#2110=AXIS2_PLACEMENT_3D('',#12030,#2540,#2541);
#2111=AXIS2_PLACEMENT_3D('',#12031,#2542,#2543);
#2112=AXIS2_PLACEMENT_3D('',#12032,#2544,#2545);
#2113=AXIS2_PLACEMENT_3D('',#12033,#2546,#2547);
#2114=AXIS2_PLACEMENT_3D('',#12034,#2548,#2549);
#2115=AXIS2_PLACEMENT_3D('',#12035,#2550,#2551);
#2116=AXIS2_PLACEMENT_3D('',#12036,#2552,#2553);
#2117=AXIS2_PLACEMENT_3D('',#12038,#2554,#2555);
#2118=AXIS2_PLACEMENT_3D('',#12040,#2556,#2557);
#2119=AXIS2_PLACEMENT_3D('',#12041,#2558,#2559);
#2120=AXIS2_PLACEMENT_3D('',#12042,#2560,#2561);
#2121=AXIS2_PLACEMENT_3D('',#12044,#2562,#2563);
#2122=AXIS2_PLACEMENT_3D('',#12046,#2564,#2565);
#2123=AXIS2_PLACEMENT_3D('',#12047,#2566,#2567);
#2124=AXIS2_PLACEMENT_3D('',#12048,#2568,#2569);
#2125=AXIS2_PLACEMENT_3D('',#12050,#2570,#2571);
#2126=AXIS2_PLACEMENT_3D('',#12053,#2573,#2574);
#2127=AXIS2_PLACEMENT_3D('',#12054,#2575,#2576);
#2128=AXIS2_PLACEMENT_3D('',#12056,#2578,#2579);
#2129=AXIS2_PLACEMENT_3D('',#12057,#2580,#2581);
#2130=AXIS2_PLACEMENT_3D('',#12058,#2582,#2583);
#2131=AXIS2_PLACEMENT_3D('',#12059,#2584,#2585);
#2132=AXIS2_PLACEMENT_3D('',#12060,#2586,#2587);
#2133=AXIS2_PLACEMENT_3D('',#12062,#2588,#2589);
#2134=AXIS2_PLACEMENT_3D('',#12065,#2591,#2592);
#2135=AXIS2_PLACEMENT_3D('',#12066,#2593,#2594);
#2136=AXIS2_PLACEMENT_3D('',#12068,#2595,#2596);
#2137=AXIS2_PLACEMENT_3D('',#12071,#2598,#2599);
#2138=AXIS2_PLACEMENT_3D('',#12072,#2600,#2601);
#2139=AXIS2_PLACEMENT_3D('',#12075,#2602,#2603);
#2140=AXIS2_PLACEMENT_3D('',#12079,#2605,#2606);
#2141=AXIS2_PLACEMENT_3D('',#12081,#2608,#2609);
#2142=AXIS2_PLACEMENT_3D('',#12084,#2610,#2611);
#2143=AXIS2_PLACEMENT_3D('',#12088,#2613,#2614);
#2144=AXIS2_PLACEMENT_3D('',#12090,#2616,#2617);
#2145=AXIS2_PLACEMENT_3D('',#12093,#2620,#2621);
#2146=AXIS2_PLACEMENT_3D('',#12095,#2623,#2624);
#2147=AXIS2_PLACEMENT_3D('',#12097,#2626,#2627);
#2148=AXIS2_PLACEMENT_3D('',#12098,#2628,#2629);
#2149=AXIS2_PLACEMENT_3D('',#12099,#2630,#2631);
#2150=AXIS2_PLACEMENT_3D('',#12100,#2632,#2633);
#2151=AXIS2_PLACEMENT_3D('',#12101,#2634,#2635);
#2152=AXIS2_PLACEMENT_3D('',#12102,#2636,#2637);
#2153=AXIS2_PLACEMENT_3D('',#12103,#2638,#2639);
#2154=AXIS2_PLACEMENT_3D('',#12104,#2640,#2641);
#2155=AXIS2_PLACEMENT_3D('',#12105,#2642,#2643);
#2156=AXIS2_PLACEMENT_3D('',#12106,#2644,#2645);
#2157=AXIS2_PLACEMENT_3D('',#12107,#2646,#2647);
#2158=AXIS2_PLACEMENT_3D('',#12108,#2648,#2649);
#2159=AXIS2_PLACEMENT_3D('',#12109,#2650,#2651);
#2160=DIRECTION('axis',(0.,0.,1.));
#2161=DIRECTION('refdir',(1.,0.,0.));
#2162=DIRECTION('axis',(0.,0.,1.));
#2163=DIRECTION('refdir',(1.,0.,0.));
#2164=DIRECTION('center_axis',(0.,1.,0.));
#2165=DIRECTION('ref_axis',(0.,0.,1.));
#2166=DIRECTION('center_axis',(0.,1.,0.));
#2167=DIRECTION('ref_axis',(0.,0.,1.));
#2168=DIRECTION('center_axis',(0.,1.,0.));
#2169=DIRECTION('ref_axis',(0.,0.,1.));
#2170=DIRECTION('center_axis',(-1.,0.,0.));
#2171=DIRECTION('ref_axis',(0.,0.,-1.));
#2172=DIRECTION('center_axis',(0.,-1.,0.));
#2173=DIRECTION('ref_axis',(0.,0.,1.));
#2174=DIRECTION('center_axis',(0.,1.,0.));
#2175=DIRECTION('ref_axis',(0.,0.,1.));
#2176=DIRECTION('center_axis',(0.,1.,0.));
#2177=DIRECTION('ref_axis',(0.,0.,1.));
#2178=DIRECTION('center_axis',(0.,1.,0.));
#2179=DIRECTION('ref_axis',(0.,0.,1.));
#2180=DIRECTION('center_axis',(-1.,0.,0.));
#2181=DIRECTION('ref_axis',(0.,0.,-1.));
#2182=DIRECTION('center_axis',(0.,-1.,0.));
#2183=DIRECTION('ref_axis',(0.,0.,1.));
#2184=DIRECTION('center_axis',(0.,-1.,0.));
#2185=DIRECTION('ref_axis',(0.,0.,-1.));
#2186=DIRECTION('',(0.,-1.,0.));
#2187=DIRECTION('center_axis',(0.,1.,0.));
#2188=DIRECTION('ref_axis',(0.,0.,1.));
#2189=DIRECTION('center_axis',(0.,-1.,0.));
#2190=DIRECTION('ref_axis',(0.,0.,-1.));
#2191=DIRECTION('',(0.,-1.,0.));
#2192=DIRECTION('center_axis',(0.,1.,0.));
#2193=DIRECTION('ref_axis',(0.,0.,1.));
#2194=DIRECTION('center_axis',(0.,1.,0.));
#2195=DIRECTION('ref_axis',(0.,0.,1.));
#2196=DIRECTION('center_axis',(0.,1.,0.));
#2197=DIRECTION('ref_axis',(0.,0.,1.));
#2198=DIRECTION('',(1.,0.,-7.77156117237611E-15));
#2199=DIRECTION('center_axis',(0.,1.,0.));
#2200=DIRECTION('ref_axis',(0.,0.,1.));
#2201=DIRECTION('',(-1.,0.,7.77156117237609E-15));
#2202=DIRECTION('center_axis',(0.,1.,0.));
#2203=DIRECTION('ref_axis',(0.,0.,1.));
#2204=DIRECTION('center_axis',(0.,1.,0.));
#2205=DIRECTION('ref_axis',(0.,0.,1.));
#2206=DIRECTION('',(1.,0.,-7.77156117237611E-15));
#2207=DIRECTION('center_axis',(0.,1.,0.));
#2208=DIRECTION('ref_axis',(0.,0.,1.));
#2209=DIRECTION('',(-1.,0.,7.77156117237609E-15));
#2210=DIRECTION('center_axis',(0.,-1.,0.));
#2211=DIRECTION('ref_axis',(0.,0.,-1.));
#2212=DIRECTION('',(0.,-1.,0.));
#2213=DIRECTION('center_axis',(0.,-1.,0.));
#2214=DIRECTION('ref_axis',(0.,0.,1.));
#2215=DIRECTION('',(0.,-1.,0.));
#2216=DIRECTION('center_axis',(7.77156117237609E-15,0.,1.));
#2217=DIRECTION('ref_axis',(1.,0.,-7.77156117237609E-15));
#2218=DIRECTION('',(0.,-1.,0.));
#2219=DIRECTION('',(1.,0.,-7.77156117237609E-15));
#2220=DIRECTION('center_axis',(0.,-1.,0.));
#2221=DIRECTION('ref_axis',(0.,0.,-1.));
#2222=DIRECTION('',(0.,-1.,0.));
#2223=DIRECTION('center_axis',(0.,-1.,0.));
#2224=DIRECTION('ref_axis',(0.,0.,1.));
#2225=DIRECTION('center_axis',(-7.77156117237611E-15,0.,-1.));
#2226=DIRECTION('ref_axis',(-1.,0.,7.77156117237611E-15));
#2227=DIRECTION('',(-1.,0.,7.77156117237611E-15));
#2228=DIRECTION('center_axis',(1.,0.,-7.77156117237609E-15));
#2229=DIRECTION('ref_axis',(-7.77156117237609E-15,0.,-1.));
#2230=DIRECTION('center_axis',(1.,0.,-6.93889390390722E-15));
#2231=DIRECTION('ref_axis',(-6.93889390390722E-15,0.,-1.));
#2232=DIRECTION('center_axis',(-1.,0.,0.));
#2233=DIRECTION('ref_axis',(0.,0.,1.));
#2234=DIRECTION('center_axis',(0.,1.,0.));
#2235=DIRECTION('ref_axis',(0.,0.,1.));
#2236=DIRECTION('center_axis',(1.,0.,0.));
#2237=DIRECTION('ref_axis',(0.,0.,-1.));
#2238=DIRECTION('center_axis',(0.,1.,0.));
#2239=DIRECTION('ref_axis',(0.,0.,1.));
#2240=DIRECTION('center_axis',(-1.,-6.93889390390723E-15,0.));
#2241=DIRECTION('ref_axis',(6.93889390390723E-15,-1.,0.));
#2242=DIRECTION('center_axis',(-1.,0.,7.77156117237611E-15));
#2243=DIRECTION('ref_axis',(7.77156117237611E-15,0.,1.));
#2244=DIRECTION('axis',(0.,0.,1.));
#2245=DIRECTION('refdir',(1.,0.,0.));
#2246=DIRECTION('center_axis',(0.,1.,0.));
#2247=DIRECTION('ref_axis',(0.,0.,1.));
#2248=DIRECTION('center_axis',(0.,-1.,0.));
#2249=DIRECTION('ref_axis',(0.,0.,-1.));
#2250=DIRECTION('',(0.,1.,0.));
#2251=DIRECTION('center_axis',(0.,1.,0.));
#2252=DIRECTION('ref_axis',(0.,0.,1.));
#2253=DIRECTION('',(0.,1.,0.));
#2254=DIRECTION('',(0.,-1.,0.));
#2255=DIRECTION('',(0.,-1.,0.));
#2256=DIRECTION('center_axis',(0.,-1.,0.));
#2257=DIRECTION('ref_axis',(0.,0.,-1.));
#2258=DIRECTION('',(0.472839131639098,0.,0.881148770407576));
#2259=DIRECTION('',(-1.,0.,0.));
#2260=DIRECTION('center_axis',(0.,-1.,0.));
#2261=DIRECTION('ref_axis',(0.,0.,-1.));
#2262=DIRECTION('',(-1.,0.,0.));
#2263=DIRECTION('',(0.472839131639098,0.,0.881148770407576));
#2264=DIRECTION('center_axis',(-0.881148770407576,0.,0.472839131639098));
#2265=DIRECTION('ref_axis',(0.472839131639098,0.,0.881148770407576));
#2266=DIRECTION('',(0.,1.,0.));
#2267=DIRECTION('center_axis',(0.,0.,-1.));
#2268=DIRECTION('ref_axis',(-1.,0.,0.));
#2269=DIRECTION('axis',(0.,0.,1.));
#2270=DIRECTION('refdir',(1.,0.,0.));
#2271=DIRECTION('center_axis',(0.,1.,0.));
#2272=DIRECTION('ref_axis',(0.,0.,1.));
#2273=DIRECTION('center_axis',(0.,1.,0.));
#2274=DIRECTION('ref_axis',(0.,0.,1.));
#2275=DIRECTION('',(0.,1.,0.));
#2276=DIRECTION('center_axis',(0.,1.,0.));
#2277=DIRECTION('ref_axis',(0.,0.,1.));
#2278=DIRECTION('',(0.,1.,0.));
#2279=DIRECTION('',(0.,-1.,0.));
#2280=DIRECTION('',(0.,1.,0.));
#2281=DIRECTION('',(0.,-1.,0.));
#2282=DIRECTION('',(0.,-1.,0.));
#2283=DIRECTION('center_axis',(0.,-1.,0.));
#2284=DIRECTION('ref_axis',(5.55111512312576E-17,0.,-1.));
#2285=DIRECTION('center_axis',(0.,-1.,0.));
#2286=DIRECTION('ref_axis',(5.55111512312576E-17,0.,-1.));
#2287=DIRECTION('',(0.211715251599179,0.,0.977331393254251));
#2288=DIRECTION('',(-0.977331393254251,0.,0.211715251599179));
#2289=DIRECTION('center_axis',(-0.977331393254252,0.,0.211715251599179));
#2290=DIRECTION('ref_axis',(0.211715251599179,0.,0.977331393254252));
#2291=DIRECTION('',(0.,1.,0.));
#2292=DIRECTION('',(0.149706258215497,-0.707102223259955,0.691082109529645));
#2293=DIRECTION('center_axis',(-0.211715251599179,0.,-0.977331393254252));
#2294=DIRECTION('ref_axis',(-0.977331393254252,0.,0.211715251599179));
#2295=DIRECTION('axis',(0.,0.,1.));
#2296=DIRECTION('refdir',(1.,0.,0.));
#2297=DIRECTION('axis',(0.,0.,1.));
#2298=DIRECTION('refdir',(1.,0.,0.));
#2299=DIRECTION('center_axis',(0.,1.,0.));
#2300=DIRECTION('ref_axis',(1.11022302462515E-16,0.,1.));
#2301=DIRECTION('center_axis',(0.,1.,0.));
#2302=DIRECTION('ref_axis',(1.11022302462515E-16,0.,1.));
#2303=DIRECTION('',(0.,1.,0.));
#2304=DIRECTION('center_axis',(0.,1.,0.));
#2305=DIRECTION('ref_axis',(1.11022302462515E-16,0.,1.));
#2306=DIRECTION('',(0.,-1.,0.));
#2307=DIRECTION('',(0.,-1.,0.));
#2308=DIRECTION('',(0.,-1.,0.));
#2309=DIRECTION('',(0.,-1.,0.));
#2310=DIRECTION('',(0.,-1.,0.));
#2311=DIRECTION('',(0.,-1.,0.));
#2312=DIRECTION('center_axis',(0.318513611714452,0.,0.94791828717069));
#2313=DIRECTION('ref_axis',(0.94791828717069,0.,-0.318513611714452));
#2314=DIRECTION('',(-0.94791828717069,0.,0.318513611714452));
#2315=DIRECTION('',(-0.947918287170691,0.,0.318513611714451));
#2316=DIRECTION('center_axis',(0.,-1.,0.));
#2317=DIRECTION('ref_axis',(-1.11022302462515E-16,0.,-1.));
#2318=DIRECTION('',(-0.946888830122557,0.,0.321561103663262));
#2319=DIRECTION('center_axis',(0.,-1.,0.));
#2320=DIRECTION('ref_axis',(-1.11022302462515E-16,0.,-1.));
#2321=DIRECTION('',(0.946888830122557,0.,-0.321561103663262));
#2322=DIRECTION('center_axis',(-0.321561103663262,0.,-0.946888830122557));
#2323=DIRECTION('ref_axis',(-0.946888830122557,0.,0.321561103663262));
#2324=DIRECTION('axis',(0.,0.,1.));
#2325=DIRECTION('refdir',(1.,0.,0.));
#2326=DIRECTION('center_axis',(0.,1.,0.));
#2327=DIRECTION('ref_axis',(0.,0.,1.));
#2328=DIRECTION('center_axis',(0.,1.,0.));
#2329=DIRECTION('ref_axis',(0.,0.,1.));
#2330=DIRECTION('',(0.,1.,0.));
#2331=DIRECTION('center_axis',(0.,1.,0.));
#2332=DIRECTION('ref_axis',(0.,0.,1.));
#2333=DIRECTION('center_axis',(0.,1.,0.));
#2334=DIRECTION('ref_axis',(2.168404344971E-16,0.,1.));
#2335=DIRECTION('center_axis',(0.,1.,0.));
#2336=DIRECTION('ref_axis',(2.168404344971E-16,0.,1.));
#2337=DIRECTION('',(0.,1.,0.));
#2338=DIRECTION('center_axis',(0.,1.,0.));
#2339=DIRECTION('ref_axis',(2.168404344971E-16,0.,1.));
#2340=DIRECTION('',(0.,-1.,0.));
#2341=DIRECTION('',(0.,-1.,0.));
#2342=DIRECTION('',(0.,-1.,0.));
#2343=DIRECTION('center_axis',(0.,-1.,0.));
#2344=DIRECTION('ref_axis',(0.873216452631512,0.,-0.487332562890721));
#2345=DIRECTION('',(0.,-1.,0.));
#2346=DIRECTION('',(0.,-1.,0.));
#2347=DIRECTION('center_axis',(-0.989219464793322,0.,0.146440603911665));
#2348=DIRECTION('ref_axis',(0.146440603911665,0.,0.989219464793322));
#2349=DIRECTION('',(-0.146440603911672,0.,-0.989219464793321));
#2350=DIRECTION('',(-0.146440603911672,0.,-0.989219464793321));
#2351=DIRECTION('center_axis',(0.,1.,0.));
#2352=DIRECTION('ref_axis',(1.11022302462515E-16,0.,1.));
#2353=DIRECTION('',(0.873216508553205,0.,-0.487332462688615));
#2354=DIRECTION('',(-0.487332462688615,0.,-0.873216508553205));
#2355=DIRECTION('',(0.873216508553205,0.,-0.487332462688615));
#2356=DIRECTION('center_axis',(0.,1.,0.));
#2357=DIRECTION('ref_axis',(1.11022302462515E-16,0.,1.));
#2358=DIRECTION('',(0.873216508553205,0.,-0.487332462688615));
#2359=DIRECTION('',(0.873216508553205,0.,-0.487332462688615));
#2360=DIRECTION('',(0.487332462688615,0.,0.873216508553205));
#2361=DIRECTION('center_axis',(0.487332462688615,0.,0.873216508553205));
#2362=DIRECTION('ref_axis',(0.873216508553205,0.,-0.487332462688615));
#2363=DIRECTION('',(0.6174573145645,-0.707106781319327,-0.344596088925887));
#2364=DIRECTION('',(0.,-1.,0.));
#2365=DIRECTION('center_axis',(-0.487332462688615,0.,-0.873216508553205));
#2366=DIRECTION('ref_axis',(-0.873216508553205,0.,0.487332462688615));
#2367=DIRECTION('',(0.,1.,0.));
#2368=DIRECTION('center_axis',(-0.873216508553205,0.,0.487332462688615));
#2369=DIRECTION('ref_axis',(0.487332462688615,0.,0.873216508553205));
#2370=DIRECTION('axis',(0.,0.,1.));
#2371=DIRECTION('refdir',(1.,0.,0.));
#2372=DIRECTION('center_axis',(-1.,0.,0.));
#2373=DIRECTION('ref_axis',(0.,0.,1.));
#2374=DIRECTION('center_axis',(1.,0.,0.));
#2375=DIRECTION('ref_axis',(0.,0.,-1.));
#2376=DIRECTION('',(1.,0.,0.));
#2377=DIRECTION('center_axis',(1.,0.,0.));
#2378=DIRECTION('ref_axis',(0.,0.,-1.));
#2379=DIRECTION('center_axis',(-1.,0.,0.));
#2380=DIRECTION('ref_axis',(0.,0.,1.));
#2381=DIRECTION('center_axis',(1.,0.,0.));
#2382=DIRECTION('ref_axis',(0.,0.,-1.));
#2383=DIRECTION('',(1.,0.,0.));
#2384=DIRECTION('center_axis',(1.,0.,0.));
#2385=DIRECTION('ref_axis',(0.,0.,-1.));
#2386=DIRECTION('center_axis',(1.,0.,0.));
#2387=DIRECTION('ref_axis',(0.,0.,-1.));
#2388=DIRECTION('center_axis',(1.,0.,0.));
#2389=DIRECTION('ref_axis',(0.,0.,-1.));
#2390=DIRECTION('center_axis',(1.,0.,0.));
#2391=DIRECTION('ref_axis',(0.,0.,-1.));
#2392=DIRECTION('',(0.,0.,1.));
#2393=DIRECTION('',(1.,0.,0.));
#2394=DIRECTION('',(0.,0.,1.));
#2395=DIRECTION('',(1.,0.,0.));
#2396=DIRECTION('',(-0.546944138603989,0.,0.837169104331222));
#2397=DIRECTION('',(0.,-1.,0.));
#2398=DIRECTION('axis',(0.,0.,1.));
#2399=DIRECTION('refdir',(1.,0.,0.));
#2400=DIRECTION('center_axis',(-1.,2.13070711535924E-14,1.04964664071668E-11));
#2401=DIRECTION('ref_axis',(1.04964925640161E-11,0.,1.));
#2402=DIRECTION('center_axis',(2.12533623997605E-14,1.,-2.83106871279414E-15));
#2403=DIRECTION('ref_axis',(8.97372454122798E-12,2.83106871260342E-15,1.));
#2404=DIRECTION('center_axis',(2.12533623997605E-14,1.,-2.83106871279414E-15));
#2405=DIRECTION('ref_axis',(8.97372454122798E-12,2.83106871260342E-15,1.));
#2406=DIRECTION('center_axis',(1.,-2.13070711535924E-14,-1.04964664071668E-11));
#2407=DIRECTION('ref_axis',(1.04964664071668E-11,1.23320016381195E-30,1.));
#2408=DIRECTION('center_axis',(-8.06361698590839E-12,0.638630771867137,
-0.769513311921493));
#2409=DIRECTION('ref_axis',(5.19723153402649E-12,0.769513311921493,0.638630771867137));
#2410=DIRECTION('center_axis',(4.51901948662213E-14,0.369697847569671,-0.929152033578118));
#2411=DIRECTION('ref_axis',(0.0324999339408396,0.928661197510084,0.369502550103484));
#2412=DIRECTION('center_axis',(-1.03853394700108E-11,0.143112919231812,
-0.989706366731542));
#2413=DIRECTION('ref_axis',(-7.02048013174369E-27,0.989706366731542,0.143112919231812));
#2414=DIRECTION('center_axis',(0.103812281246273,-0.983494881238285,0.148191864960724));
#2415=DIRECTION('ref_axis',(0.781565304323041,-0.0114833506200699,-0.623717730818172));
#2416=DIRECTION('center_axis',(0.220700126149881,0.458860340274016,0.860661746821038));
#2417=DIRECTION('ref_axis',(6.19011699821459E-17,-0.882420731745959,0.470461105921548));
#2418=DIRECTION('center_axis',(-9.28642086322632E-15,0.369697847569618,
-0.929152033578139));
#2419=DIRECTION('ref_axis',(-1.89840727556356E-30,0.929152033578139,0.369697847569618));
#2420=DIRECTION('center_axis',(1.22926249344571E-14,-0.369697847569616,
0.92915203357814));
#2421=DIRECTION('ref_axis',(-6.3986981584535E-29,0.92915203357814,0.369697847569616));
#2422=DIRECTION('center_axis',(0.0984311714245096,0.0472114241352603,0.994023332685465));
#2423=DIRECTION('ref_axis',(-0.324485630845978,-0.942758830796727,0.0769081421520186));
#2424=DIRECTION('center_axis',(1.22716376708482E-14,-0.369697847569616,
0.92915203357814));
#2425=DIRECTION('ref_axis',(-1.3530577912008E-26,-0.92915203357814,-0.369697847569616));
#2426=DIRECTION('center_axis',(1.22926249344571E-14,-0.369697847569616,
0.92915203357814));
#2427=DIRECTION('ref_axis',(-6.3986981584535E-29,0.92915203357814,0.369697847569616));
#2428=DIRECTION('',(1.,-4.13767374242821E-11,-1.64764880769037E-11));
#2429=DIRECTION('center_axis',(-1.43346686358312E-12,0.369697847570999,
-0.92915203357759));
#2430=DIRECTION('ref_axis',(-0.0324999455498311,0.928661197158793,0.369502549965296));
#2431=DIRECTION('center_axis',(9.26543359961297E-15,-0.369697847569618,
0.929152033578139));
#2432=DIRECTION('ref_axis',(-1.39344188711162E-26,-0.929152033578139,-0.369697847569618));
#2433=DIRECTION('',(-0.958764109698245,0.264067855465545,0.105069261272554));
#2434=DIRECTION('center_axis',(-9.28642086322632E-15,0.369697847569618,
-0.929152033578139));
#2435=DIRECTION('ref_axis',(-1.89840727556356E-30,0.929152033578139,0.369697847569618));
#2436=DIRECTION('center_axis',(0.220700126149881,0.458860340274016,0.860661746821038));
#2437=DIRECTION('ref_axis',(6.19011699821459E-17,-0.882420731745959,0.470461105921548));
#2438=DIRECTION('center_axis',(0.103812281246273,-0.983494881238285,0.148191864960724));
#2439=DIRECTION('ref_axis',(0.781565304323041,-0.0114833506200699,-0.623717730818172));
#2440=DIRECTION('center_axis',(0.103812281246273,-0.983494881238285,0.148191864960724));
#2441=DIRECTION('ref_axis',(0.781565304323041,-0.0114833506200699,-0.623717730818172));
#2442=DIRECTION('center_axis',(0.220700126149881,0.458860340274016,0.860661746821038));
#2443=DIRECTION('ref_axis',(1.21911388842755E-17,-0.882420731745959,0.470461105921548));
#2444=DIRECTION('center_axis',(-1.03853394700108E-11,0.143112919231812,
-0.989706366731542));
#2445=DIRECTION('ref_axis',(6.17299284843058E-27,0.989706366731542,0.143112919231812));
#2446=DIRECTION('center_axis',(-1.03853394700108E-11,0.143112919231812,
-0.989706366731542));
#2447=DIRECTION('ref_axis',(-7.02048013174369E-27,0.989706366731542,0.143112919231812));
#2448=DIRECTION('center_axis',(-8.06361698590839E-12,0.638630771867137,
-0.769513311921493));
#2449=DIRECTION('ref_axis',(5.196667977727E-12,0.769513311921493,0.638630771867137));
#2450=DIRECTION('axis',(0.,0.,1.));
#2451=DIRECTION('refdir',(1.,0.,0.));
#2452=DIRECTION('center_axis',(-1.77763333866942E-31,1.,8.62816615085482E-32));
#2453=DIRECTION('ref_axis',(2.87582171275097E-62,-8.62816615085482E-32,
1.));
#2454=DIRECTION('center_axis',(-1.77763333866942E-31,1.,8.62816615085482E-32));
#2455=DIRECTION('ref_axis',(2.87582171275097E-62,-8.62816615085482E-32,
1.));
#2456=DIRECTION('',(-1.77763333866942E-31,1.,8.62816615085482E-32));
#2457=DIRECTION('center_axis',(-1.77763333866942E-31,1.,8.62816615085482E-32));
#2458=DIRECTION('ref_axis',(1.53377158013385E-62,-8.62816615085482E-32,
1.));
#2459=DIRECTION('',(1.77763333866942E-31,-1.,-8.62816615085482E-32));
#2460=DIRECTION('',(1.77763333866942E-31,-1.,-8.62816615085482E-32));
#2461=DIRECTION('',(1.77763333866942E-31,-1.,-8.62816615085482E-32));
#2462=DIRECTION('',(1.77763333866942E-31,-1.,-8.62816615085482E-32));
#2463=DIRECTION('',(1.77763333866942E-31,-1.,-8.62816615085482E-32));
#2464=DIRECTION('center_axis',(-1.77763333866942E-31,1.,-7.54964538199795E-32));
#2465=DIRECTION('ref_axis',(2.67771827758074E-79,7.54964538199795E-32,1.));
#2466=DIRECTION('center_axis',(-1.77763333866942E-31,1.,-7.54964538199795E-32));
#2467=DIRECTION('ref_axis',(2.67771827758074E-79,7.54964538199795E-32,1.));
#2468=DIRECTION('axis',(0.,0.,1.));
#2469=DIRECTION('refdir',(1.,0.,0.));
#2470=DIRECTION('center_axis',(0.,1.,0.));
#2471=DIRECTION('ref_axis',(0.,0.,1.));
#2472=DIRECTION('center_axis',(0.,1.,0.));
#2473=DIRECTION('ref_axis',(0.,0.,1.));
#2474=DIRECTION('center_axis',(0.,1.,0.));
#2475=DIRECTION('ref_axis',(0.,0.,1.));
#2476=DIRECTION('center_axis',(-1.,0.,0.));
#2477=DIRECTION('ref_axis',(0.,0.,-1.));
#2478=DIRECTION('center_axis',(0.,-1.,0.));
#2479=DIRECTION('ref_axis',(0.,0.,1.));
#2480=DIRECTION('center_axis',(0.,1.,0.));
#2481=DIRECTION('ref_axis',(0.,0.,1.));
#2482=DIRECTION('center_axis',(0.,1.,0.));
#2483=DIRECTION('ref_axis',(0.,0.,1.));
#2484=DIRECTION('center_axis',(0.,1.,0.));
#2485=DIRECTION('ref_axis',(0.,0.,1.));
#2486=DIRECTION('center_axis',(-1.,0.,0.));
#2487=DIRECTION('ref_axis',(0.,0.,-1.));
#2488=DIRECTION('center_axis',(0.,-1.,0.));
#2489=DIRECTION('ref_axis',(0.,0.,1.));
#2490=DIRECTION('center_axis',(0.,-1.,0.));
#2491=DIRECTION('ref_axis',(0.,0.,-1.));
#2492=DIRECTION('',(0.,-1.,0.));
#2493=DIRECTION('center_axis',(0.,1.,0.));
#2494=DIRECTION('ref_axis',(0.,0.,1.));
#2495=DIRECTION('center_axis',(0.,-1.,0.));
#2496=DIRECTION('ref_axis',(0.,0.,-1.));
#2497=DIRECTION('',(0.,-1.,0.));
#2498=DIRECTION('center_axis',(0.,1.,0.));
#2499=DIRECTION('ref_axis',(0.,0.,1.));
#2500=DIRECTION('center_axis',(0.,1.,0.));
#2501=DIRECTION('ref_axis',(0.,0.,1.));
#2502=DIRECTION('center_axis',(0.,1.,0.));
#2503=DIRECTION('ref_axis',(0.,0.,1.));
#2504=DIRECTION('',(1.,0.,-7.77156117237611E-15));
#2505=DIRECTION('center_axis',(0.,1.,0.));
#2506=DIRECTION('ref_axis',(0.,0.,1.));
#2507=DIRECTION('',(-1.,0.,7.77156117237609E-15));
#2508=DIRECTION('center_axis',(0.,1.,0.));
#2509=DIRECTION('ref_axis',(0.,0.,1.));
#2510=DIRECTION('center_axis',(0.,1.,0.));
#2511=DIRECTION('ref_axis',(0.,0.,1.));
#2512=DIRECTION('',(1.,0.,-7.77156117237611E-15));
#2513=DIRECTION('center_axis',(0.,1.,0.));
#2514=DIRECTION('ref_axis',(0.,0.,1.));
#2515=DIRECTION('',(-1.,0.,7.77156117237609E-15));
#2516=DIRECTION('center_axis',(0.,-1.,0.));
#2517=DIRECTION('ref_axis',(0.,0.,-1.));
#2518=DIRECTION('',(0.,-1.,0.));
#2519=DIRECTION('center_axis',(0.,-1.,0.));
#2520=DIRECTION('ref_axis',(0.,0.,1.));
#2521=DIRECTION('',(0.,-1.,0.));
#2522=DIRECTION('center_axis',(7.77156117237609E-15,0.,1.));
#2523=DIRECTION('ref_axis',(1.,0.,-7.77156117237609E-15));
#2524=DIRECTION('',(0.,-1.,0.));
#2525=DIRECTION('',(1.,0.,-7.77156117237609E-15));
#2526=DIRECTION('center_axis',(0.,-1.,0.));
#2527=DIRECTION('ref_axis',(0.,0.,-1.));
#2528=DIRECTION('',(0.,-1.,0.));
#2529=DIRECTION('center_axis',(0.,-1.,0.));
#2530=DIRECTION('ref_axis',(0.,0.,1.));
#2531=DIRECTION('center_axis',(-7.77156117237611E-15,0.,-1.));
#2532=DIRECTION('ref_axis',(-1.,0.,7.77156117237611E-15));
#2533=DIRECTION('',(-1.,0.,7.77156117237611E-15));
#2534=DIRECTION('center_axis',(1.,0.,-7.77156117237609E-15));
#2535=DIRECTION('ref_axis',(-7.77156117237609E-15,0.,-1.));
#2536=DIRECTION('center_axis',(1.,0.,-6.93889390390722E-15));
#2537=DIRECTION('ref_axis',(-6.93889390390722E-15,0.,-1.));
#2538=DIRECTION('center_axis',(-1.,0.,0.));
#2539=DIRECTION('ref_axis',(0.,0.,1.));
#2540=DIRECTION('center_axis',(0.,1.,0.));
#2541=DIRECTION('ref_axis',(0.,0.,1.));
#2542=DIRECTION('center_axis',(1.,0.,0.));
#2543=DIRECTION('ref_axis',(0.,0.,-1.));
#2544=DIRECTION('center_axis',(0.,1.,0.));
#2545=DIRECTION('ref_axis',(0.,0.,1.));
#2546=DIRECTION('center_axis',(-1.,-6.93889390390723E-15,0.));
#2547=DIRECTION('ref_axis',(6.93889390390723E-15,-1.,0.));
#2548=DIRECTION('center_axis',(-1.,0.,7.77156117237611E-15));
#2549=DIRECTION('ref_axis',(7.77156117237611E-15,0.,1.));
#2550=DIRECTION('axis',(0.,0.,1.));
#2551=DIRECTION('refdir',(1.,0.,0.));
#2552=DIRECTION('center_axis',(-4.27556447653966E-32,1.97215226305253E-31,
1.));
#2553=DIRECTION('ref_axis',(1.,1.68641283164694E-62,0.));
#2554=DIRECTION('center_axis',(-4.27556447653966E-32,1.97215226305253E-31,
1.));
#2555=DIRECTION('ref_axis',(1.,1.76237737361302E-62,4.27556447653966E-32));
#2556=DIRECTION('center_axis',(1.22464679914735E-16,-1.,1.97215226305253E-31));
#2557=DIRECTION('ref_axis',(-1.,-1.22464679914735E-16,0.));
#2558=DIRECTION('center_axis',(4.27556447653966E-32,-1.97215226305253E-31,
-1.));
#2559=DIRECTION('ref_axis',(1.,8.88178419700125E-16,4.27556447653964E-32));
#2560=DIRECTION('center_axis',(-4.27556447653966E-32,1.97215226305253E-31,
1.));
#2561=DIRECTION('ref_axis',(1.,1.68641283164694E-62,0.));
#2562=DIRECTION('center_axis',(-4.27556447653966E-32,1.97215226305253E-31,
1.));
#2563=DIRECTION('ref_axis',(1.,8.4320641582347E-63,4.27556447653966E-32));
#2564=DIRECTION('center_axis',(1.22464679914735E-16,-1.,1.97215226305253E-31));
#2565=DIRECTION('ref_axis',(-1.,-1.22464679914735E-16,0.));
#2566=DIRECTION('center_axis',(4.27556447653966E-32,-1.97215226305253E-31,
-1.));
#2567=DIRECTION('ref_axis',(1.,8.4320641582347E-63,4.27556447653966E-32));
#2568=DIRECTION('center_axis',(4.27556447653966E-32,-1.97215226305253E-31,
-1.));
#2569=DIRECTION('ref_axis',(-1.,-8.4320641582347E-63,-4.27556447653966E-32));
#2570=DIRECTION('center_axis',(-4.27556447653966E-32,1.97215226305253E-31,
1.));
#2571=DIRECTION('ref_axis',(1.,1.76237737361302E-62,4.27556447653966E-32));
#2572=DIRECTION('',(-4.27556447653966E-32,1.97215226305253E-31,1.));
#2573=DIRECTION('center_axis',(-4.27556447653966E-32,1.97215226305253E-31,
1.));
#2574=DIRECTION('ref_axis',(1.,8.4320641582347E-63,4.27556447653966E-32));
#2575=DIRECTION('center_axis',(-4.27556447653966E-32,1.97215226305253E-31,
1.));
#2576=DIRECTION('ref_axis',(1.,8.4320641582347E-63,4.27556447653966E-32));
#2577=DIRECTION('',(4.27556447653966E-32,-1.97215226305253E-31,-1.));
#2578=DIRECTION('center_axis',(4.66075046541711E-32,1.97215226305253E-31,
1.));
#2579=DIRECTION('ref_axis',(1.,1.18072616964182E-79,-4.66075046541711E-32));
#2580=DIRECTION('center_axis',(4.66075046541711E-32,1.97215226305253E-31,
1.));
#2581=DIRECTION('ref_axis',(1.,1.18072616964182E-79,-4.66075046541711E-32));
#2582=DIRECTION('center_axis',(4.66075046541711E-32,1.97215226305253E-31,
1.));
#2583=DIRECTION('ref_axis',(1.,1.18072616964182E-79,-4.66075046541711E-32));
#2584=DIRECTION('axis',(0.,0.,1.));
#2585=DIRECTION('refdir',(1.,0.,0.));
#2586=DIRECTION('center_axis',(0.,-1.,0.));
#2587=DIRECTION('ref_axis',(0.,0.,-1.));
#2588=DIRECTION('center_axis',(0.,1.,0.));
#2589=DIRECTION('ref_axis',(0.,0.,1.));
#2590=DIRECTION('',(0.,-1.,0.));
#2591=DIRECTION('center_axis',(0.,1.,0.));
#2592=DIRECTION('ref_axis',(0.,0.,1.));
#2593=DIRECTION('center_axis',(0.,-1.,0.));
#2594=DIRECTION('ref_axis',(0.,0.,-1.));
#2595=DIRECTION('center_axis',(0.,1.,0.));
#2596=DIRECTION('ref_axis',(0.,0.,1.));
#2597=DIRECTION('',(0.,-1.,0.));
#2598=DIRECTION('center_axis',(0.,1.,0.));
#2599=DIRECTION('ref_axis',(0.,0.,1.));
#2600=DIRECTION('center_axis',(0.,1.,0.));
#2601=DIRECTION('ref_axis',(0.,0.,1.));
#2602=DIRECTION('center_axis',(0.,1.,0.));
#2603=DIRECTION('ref_axis',(0.,0.,1.));
#2604=DIRECTION('',(-1.,0.,-2.42861286636752E-16));
#2605=DIRECTION('center_axis',(0.,1.,0.));
#2606=DIRECTION('ref_axis',(0.,0.,1.));
#2607=DIRECTION('',(1.,0.,-1.38777878078144E-16));
#2608=DIRECTION('center_axis',(0.,1.,0.));
#2609=DIRECTION('ref_axis',(0.,0.,1.));
#2610=DIRECTION('center_axis',(0.,1.,0.));
#2611=DIRECTION('ref_axis',(0.,0.,1.));
#2612=DIRECTION('',(1.,0.,-1.38777878078144E-16));
#2613=DIRECTION('center_axis',(0.,1.,0.));
#2614=DIRECTION('ref_axis',(0.,0.,1.));
#2615=DIRECTION('',(-1.,0.,-2.42861286636752E-16));
#2616=DIRECTION('center_axis',(0.,-1.,0.));
#2617=DIRECTION('ref_axis',(0.,0.,-1.));
#2618=DIRECTION('',(0.,-1.,0.));
#2619=DIRECTION('',(0.,-1.,0.));
#2620=DIRECTION('center_axis',(-2.42861286636752E-16,0.,1.));
#2621=DIRECTION('ref_axis',(1.,0.,2.42861286636752E-16));
#2622=DIRECTION('',(0.,-1.,0.));
#2623=DIRECTION('center_axis',(0.,-1.,0.));
#2624=DIRECTION('ref_axis',(0.,0.,-1.));
#2625=DIRECTION('',(0.,-1.,0.));
#2626=DIRECTION('center_axis',(-1.38777878078144E-16,0.,-1.));
#2627=DIRECTION('ref_axis',(-1.,0.,1.38777878078144E-16));
#2628=DIRECTION('',(0.,0.,1.));
#2629=DIRECTION('',(1.,0.,0.));
#2630=DIRECTION('',(0.,0.,1.));
#2631=DIRECTION('',(1.,0.,0.));
#2632=DIRECTION('',(3.49433275961973E-17,-1.,-1.17373598748277E-16));
#2633=DIRECTION('',(-0.999760008818507,-3.23636163300894E-17,-0.0219071852874454));
#2634=DIRECTION('',(0.,0.,1.));
#2635=DIRECTION('',(1.,0.,0.));
#2636=DIRECTION('',(0.766591083091299,0.,0.642135586402833));
#2637=DIRECTION('',(0.642135586402833,0.,-0.766591083091299));
#2638=DIRECTION('',(0.323521451769555,0.,0.946220835875495));
#2639=DIRECTION('',(0.946220835875495,0.,-0.323521451769555));
#2640=DIRECTION('',(-0.992631319332961,1.04964664071669E-11,-0.1211736930167));
#2641=DIRECTION('',(-1.04217031545792E-11,-1.,-1.25074553203183E-12));
#2642=DIRECTION('',(0.556347891604863,1.42362526751793E-17,0.830949471091248));
#2643=DIRECTION('',(-0.830949471091248,-2.54938842133024E-17,0.556347891604863));
#2644=DIRECTION('',(0.,6.98296267768627E-15,-1.));
#2645=DIRECTION('',(1.,0.,0.));
#2646=DIRECTION('',(-7.61196661258623E-15,0.,-1.));
#2647=DIRECTION('',(-1.,0.,7.61196661258623E-15));
#2648=DIRECTION('',(0.,-1.,0.));
#2649=DIRECTION('',(1.,0.,0.));
#2650=DIRECTION('',(0.,0.,1.));
#2651=DIRECTION('',(1.,0.,0.));
#2652=CARTESIAN_POINT('',(0.,0.,0.));
#2653=CARTESIAN_POINT('',(0.,0.,0.));
#2654=CARTESIAN_POINT('Origin',(-83.4892602927113,2.,28.6344795489034));
#2655=CARTESIAN_POINT('',(-83.4892602927113,2.,30.6344795489034));
#2656=CARTESIAN_POINT('',(-83.4892602927113,2.,26.6344795489034));
#2657=CARTESIAN_POINT('Origin',(-83.4892602927113,2.,28.6344795489034));
#2658=CARTESIAN_POINT('Origin',(-83.4892602927113,2.,28.6344795489034));
#2659=CARTESIAN_POINT('',(-83.4892602927113,2.5,26.1344795489034));
#2660=CARTESIAN_POINT('Origin',(-83.4892602927113,2.,26.1344795489034));
#2661=CARTESIAN_POINT('Origin',(-83.4892602927113,2.5,28.6344795489034));
#2662=CARTESIAN_POINT('Origin',(16.5107397072887,2.,28.6344795489026));
#2663=CARTESIAN_POINT('',(16.5107397072887,2.,30.6344795489026));
#2664=CARTESIAN_POINT('',(16.5107397072887,2.,26.6344795489026));
#2665=CARTESIAN_POINT('Origin',(16.5107397072887,2.,28.6344795489026));
#2666=CARTESIAN_POINT('Origin',(16.5107397072887,2.,28.6344795489026));
#2667=CARTESIAN_POINT('',(16.5107397072887,2.5,26.1344795489026));
#2668=CARTESIAN_POINT('Origin',(16.5107397072887,2.,26.1344795489026));
#2669=CARTESIAN_POINT('Origin',(16.5107397072887,2.5,28.6344795489026));
#2670=CARTESIAN_POINT('Origin',(16.5107397072887,2.5,28.6344795489026));
#2671=CARTESIAN_POINT('',(16.5107397072887,0.,30.6344795489026));
#2672=CARTESIAN_POINT('',(16.5107397072887,2.5,30.6344795489026));
#2673=CARTESIAN_POINT('Origin',(16.5107397072887,0.,28.6344795489026));
#2674=CARTESIAN_POINT('Origin',(-83.4892602927113,2.5,28.6344795489034));
#2675=CARTESIAN_POINT('',(-83.4892602927113,0.,30.6344795489034));
#2676=CARTESIAN_POINT('',(-83.4892602927113,2.5,30.6344795489034));
#2677=CARTESIAN_POINT('Origin',(-83.4892602927113,0.,28.6344795489034));
#2678=CARTESIAN_POINT('Origin',(16.5107397072887,2.5,28.6344795489026));
#2679=CARTESIAN_POINT('',(-83.4892602927114,2.5,16.8621786589128));
#2680=CARTESIAN_POINT('',(-83.4892602927112,2.5,40.4067804388939));
#2681=CARTESIAN_POINT('Origin',(-83.4892602927113,2.5,28.6344795489034));
#2682=CARTESIAN_POINT('',(16.5107397072887,2.5,40.4067804388932));
#2683=CARTESIAN_POINT('',(16.5107397072887,2.5,40.4067804388932));
#2684=CARTESIAN_POINT('',(16.5107397072887,2.5,16.862178658912));
#2685=CARTESIAN_POINT('Origin',(16.5107397072887,2.5,28.6344795489026));
#2686=CARTESIAN_POINT('',(-83.4892602927114,2.5,16.8621786589128));
#2687=CARTESIAN_POINT('Origin',(16.5107397072887,0.,28.6344795489026));
#2688=CARTESIAN_POINT('',(16.5107397072887,0.,40.9067804388932));
#2689=CARTESIAN_POINT('',(16.5107397072887,0.,16.362178658912));
#2690=CARTESIAN_POINT('Origin',(16.5107397072887,0.,28.6344795489026));
#2691=CARTESIAN_POINT('',(-83.4892602927112,0.,40.9067804388939));
#2692=CARTESIAN_POINT('',(16.5107397072887,0.,40.9067804388932));
#2693=CARTESIAN_POINT('',(-83.4892602927114,0.,16.3621786589128));
#2694=CARTESIAN_POINT('Origin',(-83.4892602927113,0.,28.6344795489034));
#2695=CARTESIAN_POINT('',(16.5107397072887,0.,16.362178658912));
#2696=CARTESIAN_POINT('Origin',(16.5107397072887,2.5,28.6344795489026));
#2697=CARTESIAN_POINT('',(16.5107397072887,2.,16.362178658912));
#2698=CARTESIAN_POINT('',(16.5107397072887,2.5,16.362178658912));
#2699=CARTESIAN_POINT('',(16.5107397072887,2.,40.9067804388932));
#2700=CARTESIAN_POINT('Origin',(16.5107397072887,2.,28.6344795489026));
#2701=CARTESIAN_POINT('',(16.5107397072887,2.5,40.9067804388932));
#2702=CARTESIAN_POINT('Origin',(16.5107397072887,2.5,16.362178658912));
#2703=CARTESIAN_POINT('',(-83.4892602927114,2.,16.3621786589128));
#2704=CARTESIAN_POINT('',(-83.4892602927114,2.5,16.3621786589128));
#2705=CARTESIAN_POINT('',(16.5107397072887,2.,16.362178658912));
#2706=CARTESIAN_POINT('Origin',(-83.4892602927113,2.5,28.6344795489034));
#2707=CARTESIAN_POINT('',(-83.4892602927112,2.,40.9067804388939));
#2708=CARTESIAN_POINT('',(-83.4892602927112,2.5,40.9067804388939));
#2709=CARTESIAN_POINT('Origin',(-83.4892602927113,2.,28.6344795489034));
#2710=CARTESIAN_POINT('Origin',(16.5107397072887,2.5,40.9067804388932));
#2711=CARTESIAN_POINT('',(-83.4892602927112,2.,40.9067804388939));
#2712=CARTESIAN_POINT('Origin',(16.5107397072886,2.,16.862178658912));
#2713=CARTESIAN_POINT('Origin',(16.5107397072887,2.,16.862178658912));
#2714=CARTESIAN_POINT('Origin',(-83.4892602927114,2.,16.8621786589128));
#2715=CARTESIAN_POINT('Origin',(-83.4892602927113,2.,28.6344795489034));
#2716=CARTESIAN_POINT('Origin',(-83.4892602927112,2.,40.4067804388939));
#2717=CARTESIAN_POINT('Origin',(16.5107397072887,2.,28.6344795489026));
#2718=CARTESIAN_POINT('Origin',(16.5107397072887,2.,40.4067804388932));
#2719=CARTESIAN_POINT('Origin',(16.5107397072888,2.,40.4067804388932));
#2720=CARTESIAN_POINT('',(0.,0.,0.));
#2721=CARTESIAN_POINT('Origin',(42.7532306583709,-0.000750036417118335,
-2.95713890544537));
#2722=CARTESIAN_POINT('',(42.7532306583709,0.,-4.95713890544537));
#2723=CARTESIAN_POINT('Origin',(42.7532306583709,0.,-2.95713890544537));
#2724=CARTESIAN_POINT('',(42.7532306583709,1.5,-4.95713890544537));
#2725=CARTESIAN_POINT('',(42.7532306583709,-0.000750036417118335,-4.95713890544537));
#2726=CARTESIAN_POINT('Origin',(42.7532306583709,1.5,-2.95713890544537));
#2727=CARTESIAN_POINT('Ctrl Pts',(25.9188618862632,1.5,3.73655812708952));
#2728=CARTESIAN_POINT('Ctrl Pts',(25.9188618862632,-0.66,3.73655812708952));
#2729=CARTESIAN_POINT('Ctrl Pts',(26.0838087555079,1.5,3.69528174729993));
#2730=CARTESIAN_POINT('Ctrl Pts',(26.0838087555079,-0.66,3.69528174729993));
#2731=CARTESIAN_POINT('Ctrl Pts',(26.7414333467756,1.5,3.66889628312799));
#2732=CARTESIAN_POINT('Ctrl Pts',(26.7414333467756,-0.66,3.66889628312799));
#2733=CARTESIAN_POINT('Ctrl Pts',(27.3011855299882,1.5,5.05266376239426));
#2734=CARTESIAN_POINT('Ctrl Pts',(27.3011855299882,-0.66,5.05266376239426));
#2735=CARTESIAN_POINT('Ctrl Pts',(27.9697213442539,1.5,6.64187212001263));
#2736=CARTESIAN_POINT('Ctrl Pts',(27.9697213442539,-0.66,6.64187212001263));
#2737=CARTESIAN_POINT('Ctrl Pts',(30.0035737390622,1.5,5.70550320798981));
#2738=CARTESIAN_POINT('Ctrl Pts',(30.0035737390622,-0.66,5.70550320798981));
#2739=CARTESIAN_POINT('Ctrl Pts',(31.8783416154944,1.5,5.75245772223251));
#2740=CARTESIAN_POINT('Ctrl Pts',(31.8783416154944,-0.66,5.75245772223251));
#2741=CARTESIAN_POINT('Ctrl Pts',(35.1844604255421,1.5,4.32025211416494));
#2742=CARTESIAN_POINT('Ctrl Pts',(35.1844604255421,-0.66,4.32025211416494));
#2743=CARTESIAN_POINT('Ctrl Pts',(40.192401529867,1.5,3.55204841770967));
#2744=CARTESIAN_POINT('Ctrl Pts',(40.192401529867,-0.66,3.55204841770967));
#2745=CARTESIAN_POINT('Ctrl Pts',(47.9284527442042,1.5,4.14235365515584));
#2746=CARTESIAN_POINT('Ctrl Pts',(47.9284527442042,-0.66,4.14235365515584));
#2747=CARTESIAN_POINT('Ctrl Pts',(51.435120996177,1.5,-7.206342921025));
#2748=CARTESIAN_POINT('Ctrl Pts',(51.435120996177,-0.66,-7.206342921025));
#2749=CARTESIAN_POINT('Ctrl Pts',(48.7532306583708,1.5,-7.95408926393385));
#2750=CARTESIAN_POINT('Ctrl Pts',(48.7532306583708,-0.66,-7.95408926393385));
#2751=CARTESIAN_POINT('',(25.9188618861119,1.5,3.73655812712738));
#2752=CARTESIAN_POINT('',(48.7532306583709,1.5,-7.95408926393383));
#2753=CARTESIAN_POINT('Ctrl Pts',(25.9188618862632,1.5,3.73655812708952));
#2754=CARTESIAN_POINT('Ctrl Pts',(26.0838087555079,1.5,3.69528174729993));
#2755=CARTESIAN_POINT('Ctrl Pts',(26.7414333467756,1.5,3.66889628312799));
#2756=CARTESIAN_POINT('Ctrl Pts',(27.3011855299882,1.5,5.05266376239426));
#2757=CARTESIAN_POINT('Ctrl Pts',(27.9697213442539,1.5,6.64187212001263));
#2758=CARTESIAN_POINT('Ctrl Pts',(30.0035737390622,1.5,5.70550320798981));
#2759=CARTESIAN_POINT('Ctrl Pts',(31.8783416154944,1.5,5.75245772223251));
#2760=CARTESIAN_POINT('Ctrl Pts',(35.1844604255421,1.5,4.32025211416494));
#2761=CARTESIAN_POINT('Ctrl Pts',(40.192401529867,1.5,3.55204841770967));
#2762=CARTESIAN_POINT('Ctrl Pts',(47.9284527442042,1.5,4.14235365515584));
#2763=CARTESIAN_POINT('Ctrl Pts',(51.435120996177,1.5,-7.206342921025));
#2764=CARTESIAN_POINT('Ctrl Pts',(48.7532306583708,1.5,-7.95408926393385));
#2765=CARTESIAN_POINT('',(25.9188618861119,0.,3.73655812712738));
#2766=CARTESIAN_POINT('',(25.9188618861119,0.,3.73655812712738));
#2767=CARTESIAN_POINT('',(48.7532306583709,0.,-7.95408926393383));
#2768=CARTESIAN_POINT('Ctrl Pts',(25.9188618862632,0.,3.73655812708952));
#2769=CARTESIAN_POINT('Ctrl Pts',(26.0838087555079,0.,3.69528174729993));
#2770=CARTESIAN_POINT('Ctrl Pts',(26.7414333467756,0.,3.66889628312799));
#2771=CARTESIAN_POINT('Ctrl Pts',(27.3011855299882,0.,5.05266376239426));
#2772=CARTESIAN_POINT('Ctrl Pts',(27.9697213442539,0.,6.64187212001263));
#2773=CARTESIAN_POINT('Ctrl Pts',(30.0035737390622,0.,5.70550320798981));
#2774=CARTESIAN_POINT('Ctrl Pts',(31.8783416154944,0.,5.75245772223251));
#2775=CARTESIAN_POINT('Ctrl Pts',(35.1844604255421,0.,4.32025211416494));
#2776=CARTESIAN_POINT('Ctrl Pts',(40.192401529867,0.,3.55204841770967));
#2777=CARTESIAN_POINT('Ctrl Pts',(47.9284527442042,0.,4.14235365515584));
#2778=CARTESIAN_POINT('Ctrl Pts',(51.435120996177,0.,-7.206342921025));
#2779=CARTESIAN_POINT('Ctrl Pts',(48.7532306583708,0.,-7.95408926393385));
#2780=CARTESIAN_POINT('',(48.7532306583709,1.5,-7.95408926393383));
#2781=CARTESIAN_POINT('Ctrl Pts',(48.7532306583709,1.5,-7.95408926393383));
#2782=CARTESIAN_POINT('Ctrl Pts',(48.7532306583709,-0.66,-7.95408926393383));
#2783=CARTESIAN_POINT('Ctrl Pts',(36.6068452277914,1.5,-11.3406614728137));
#2784=CARTESIAN_POINT('Ctrl Pts',(36.6068452277914,-0.66,-11.3406614728137));
#2785=CARTESIAN_POINT('Ctrl Pts',(39.4535021242481,1.5,-4.7454968822424));
#2786=CARTESIAN_POINT('Ctrl Pts',(39.4535021242481,-0.66,-4.7454968822424));
#2787=CARTESIAN_POINT('Ctrl Pts',(31.9355686583357,1.5,-5.55619061474896));
#2788=CARTESIAN_POINT('Ctrl Pts',(31.9355686583357,-0.66,-5.55619061474896));
#2789=CARTESIAN_POINT('Ctrl Pts',(28.7242328419571,1.5,-5.63921626360694));
#2790=CARTESIAN_POINT('Ctrl Pts',(28.7242328419571,-0.66,-5.63921626360694));
#2791=CARTESIAN_POINT('Ctrl Pts',(28.0628515535919,1.5,-8.54333666903048));
#2792=CARTESIAN_POINT('Ctrl Pts',(28.0628515535919,-0.66,-8.54333666903048));
#2793=CARTESIAN_POINT('',(28.0628515535919,0.,-8.54333666903048));
#2794=CARTESIAN_POINT('Ctrl Pts',(48.7532306583709,0.,-7.95408926393383));
#2795=CARTESIAN_POINT('Ctrl Pts',(36.6068452277914,0.,-11.3406614728137));
#2796=CARTESIAN_POINT('Ctrl Pts',(39.4535021242481,0.,-4.7454968822424));
#2797=CARTESIAN_POINT('Ctrl Pts',(31.9355686583357,0.,-5.55619061474896));
#2798=CARTESIAN_POINT('Ctrl Pts',(28.7242328419571,0.,-5.63921626360694));
#2799=CARTESIAN_POINT('Ctrl Pts',(28.0628515535919,0.,-8.54333666903048));
#2800=CARTESIAN_POINT('',(28.0628515535919,1.5,-8.54333666903048));
#2801=CARTESIAN_POINT('',(28.0628515535919,1.5,-8.54333666903048));
#2802=CARTESIAN_POINT('Ctrl Pts',(48.7532306583709,1.5,-7.95408926393383));
#2803=CARTESIAN_POINT('Ctrl Pts',(36.6068452277914,1.5,-11.3406614728137));
#2804=CARTESIAN_POINT('Ctrl Pts',(39.4535021242481,1.5,-4.7454968822424));
#2805=CARTESIAN_POINT('Ctrl Pts',(31.9355686583357,1.5,-5.55619061474896));
#2806=CARTESIAN_POINT('Ctrl Pts',(28.7242328419571,1.5,-5.63921626360694));
#2807=CARTESIAN_POINT('Ctrl Pts',(28.0628515535919,1.5,-8.54333666903048));
#2808=CARTESIAN_POINT('Ctrl Pts',(28.0628515535919,1.5,-8.54333666903048));
#2809=CARTESIAN_POINT('Ctrl Pts',(28.0628515535919,-0.660000000473272,-8.54333666903048));
#2810=CARTESIAN_POINT('Ctrl Pts',(25.2439018750637,1.5,-8.53533145112329));
#2811=CARTESIAN_POINT('Ctrl Pts',(25.2439018750637,-0.660000000473272,-8.53533145112329));
#2812=CARTESIAN_POINT('Ctrl Pts',(10.2818042790062,1.5,-8.66732731527297));
#2813=CARTESIAN_POINT('Ctrl Pts',(10.2818042790062,-0.660000000473272,-8.66732731527297));
#2814=CARTESIAN_POINT('Ctrl Pts',(-10.8727124848744,1.5,-9.29910974996734));
#2815=CARTESIAN_POINT('Ctrl Pts',(-10.8727124848744,-0.660000000473272,
-9.29910974996734));
#2816=CARTESIAN_POINT('Ctrl Pts',(-35.4046976733781,1.5,-5.36519475551457));
#2817=CARTESIAN_POINT('Ctrl Pts',(-35.4046976733781,-0.660000000473272,
-5.36519475551457));
#2818=CARTESIAN_POINT('Ctrl Pts',(-46.8925527716544,1.5,0.201186051515265));
#2819=CARTESIAN_POINT('Ctrl Pts',(-46.8925527716544,-0.660000000473272,
0.201186051515265));
#2820=CARTESIAN_POINT('Ctrl Pts',(-51.680694477123,1.5,4.4617348855033));
#2821=CARTESIAN_POINT('Ctrl Pts',(-51.680694477123,-0.660000000473272,4.4617348855033));
#2822=CARTESIAN_POINT('',(-51.6806944520712,7.01907565403559E-9,4.4617348606735));
#2823=CARTESIAN_POINT('Ctrl Pts',(28.0628515535919,0.,-8.54333666903048));
#2824=CARTESIAN_POINT('Ctrl Pts',(25.2439018750637,0.,-8.53533145112329));
#2825=CARTESIAN_POINT('Ctrl Pts',(10.2818042790062,0.,-8.66732731527297));
#2826=CARTESIAN_POINT('Ctrl Pts',(-10.8727124848744,0.,-9.29910974996734));
#2827=CARTESIAN_POINT('Ctrl Pts',(-35.4046976617966,0.,-5.36519475737177));
#2828=CARTESIAN_POINT('Ctrl Pts',(-46.892552750304,0.,0.201186041170038));
#2829=CARTESIAN_POINT('Ctrl Pts',(-51.6806944508158,0.,4.46173486209483));
#2830=CARTESIAN_POINT('',(-50.5272419105718,1.5,3.47897350344959));
#2831=CARTESIAN_POINT('Ctrl Pts',(-51.6806944612578,2.10963722047097E-8,
4.46173487138622));
#2832=CARTESIAN_POINT('Ctrl Pts',(-51.433849902908,0.328235390347009,4.24208947267881));
#2833=CARTESIAN_POINT('Ctrl Pts',(-51.1892976355325,0.648631772383023,4.03075620524778));
#2834=CARTESIAN_POINT('Ctrl Pts',(-50.9474658918659,0.961189167121584,3.82721318363075));
#2835=CARTESIAN_POINT('Ctrl Pts',(-50.806440496671,1.14345858074691,3.70851604888949));
#2836=CARTESIAN_POINT('Ctrl Pts',(-50.666339525841,1.32306219171186,3.59246881728103));
#2837=CARTESIAN_POINT('Ctrl Pts',(-50.5272419105718,1.5,3.47897350344958));
#2838=CARTESIAN_POINT('Ctrl Pts',(28.0628515535919,1.5,-8.54333666903048));
#2839=CARTESIAN_POINT('Ctrl Pts',(25.2439018750637,1.5,-8.53533145112329));
#2840=CARTESIAN_POINT('Ctrl Pts',(10.2818042790062,1.5,-8.66732731527297));
#2841=CARTESIAN_POINT('Ctrl Pts',(-10.8727124848744,1.5,-9.29910974996734));
#2842=CARTESIAN_POINT('Ctrl Pts',(-34.9052983608708,1.5,-5.4452777340667));
#2843=CARTESIAN_POINT('Ctrl Pts',(-45.9703553177735,1.5,-0.239172727476468));
#2844=CARTESIAN_POINT('Ctrl Pts',(-50.5272419105718,1.5,3.47897350344959));
#2845=CARTESIAN_POINT('Origin',(1.90003279625137,1.5,8.11589060443533));
#2846=CARTESIAN_POINT('',(21.5644964975589,1.49999999962684,4.16303199048503));
#2847=CARTESIAN_POINT('Ctrl Pts',(-50.5272419105718,1.50000000000001,3.4789735034496));
#2848=CARTESIAN_POINT('Ctrl Pts',(-50.5089293710935,1.50000000000002,3.494919364608));
#2849=CARTESIAN_POINT('Ctrl Pts',(-50.490585009579,1.50000000000002,3.51082303253495));
#2850=CARTESIAN_POINT('Ctrl Pts',(-50.472208669657,1.50000000000003,3.5266846817746));
#2851=CARTESIAN_POINT('Ctrl Pts',(-50.4314411765197,1.50000000000004,3.56187339069447));
#2852=CARTESIAN_POINT('Ctrl Pts',(-50.3905163002735,1.50000000000005,3.59685530223419));
#2853=CARTESIAN_POINT('Ctrl Pts',(-50.3494323020579,1.50000000000006,3.63163228677637));
#2854=CARTESIAN_POINT('Ctrl Pts',(-50.2671881545655,1.50000000000008,3.70125071658485));
#2855=CARTESIAN_POINT('Ctrl Pts',(-50.1842968962082,1.5000000000001,3.77005537571968));
#2856=CARTESIAN_POINT('Ctrl Pts',(-50.1007725161627,1.50000000000012,3.83803845959699));
#2857=CARTESIAN_POINT('Ctrl Pts',(-50.0171711659525,1.50000000000013,3.90608419187893));
#2858=CARTESIAN_POINT('Ctrl Pts',(-49.9328424659519,1.50000000000015,3.97337933108099));
#2859=CARTESIAN_POINT('Ctrl Pts',(-49.8480096700854,1.50000000000016,4.03975178559884));
#2860=CARTESIAN_POINT('Ctrl Pts',(-49.763130854313,1.50000000000017,4.10616024569771));
#2861=CARTESIAN_POINT('Ctrl Pts',(-49.6778155128328,1.50000000000018,4.17159851421962));
#2862=CARTESIAN_POINT('Ctrl Pts',(-49.5920096605213,1.50000000000018,4.23611727603634));
#2863=CARTESIAN_POINT('Ctrl Pts',(-49.3831630067192,1.5000000000002,4.3931523400779));
#2864=CARTESIAN_POINT('Ctrl Pts',(-49.1715354999119,1.50000000000021,4.54469690390822));
#2865=CARTESIAN_POINT('Ctrl Pts',(-48.9569720150866,1.50000000000021,4.69110256404027));
#2866=CARTESIAN_POINT('Ctrl Pts',(-48.8191090810188,1.5000000000002,4.78517222312685));
#2867=CARTESIAN_POINT('Ctrl Pts',(-48.6800335406078,1.5000000000002,4.87711933779923));
#2868=CARTESIAN_POINT('Ctrl Pts',(-48.5396990336734,1.5000000000002,4.96702716533848));
#2869=CARTESIAN_POINT('Ctrl Pts',(-48.3121370230267,1.50000000000019,5.11281886300889));
#2870=CARTESIAN_POINT('Ctrl Pts',(-48.0812724142786,1.50000000000017,5.25325158941465));
#2871=CARTESIAN_POINT('Ctrl Pts',(-47.8469042857071,1.50000000000016,5.38865160350329));
#2872=CARTESIAN_POINT('Ctrl Pts',(-47.7137848477506,1.50000000000015,5.46555785302046));
#2873=CARTESIAN_POINT('Ctrl Pts',(-47.5795346580899,1.50000000000015,5.54083958227443));
#2874=CARTESIAN_POINT('Ctrl Pts',(-47.4441134822786,1.50000000000014,5.61454999218334));
#2875=CARTESIAN_POINT('Ctrl Pts',(-47.259034597612,1.50000000000013,5.71528933647368));
#2876=CARTESIAN_POINT('Ctrl Pts',(-47.0717688974148,1.50000000000013,5.81309447963658));
#2877=CARTESIAN_POINT('Ctrl Pts',(-46.8822088597417,1.50000000000013,5.90809195718259));
#2878=CARTESIAN_POINT('Ctrl Pts',(-46.8348188503235,1.50000000000013,5.9318413265691));
#2879=CARTESIAN_POINT('Ctrl Pts',(-46.7872854082889,1.50000000000013,5.95541514647583));
#2880=CARTESIAN_POINT('Ctrl Pts',(-46.7396067820982,1.50000000000013,5.97881525622759));
#2881=CARTESIAN_POINT('Ctrl Pts',(-46.7199618861861,1.50000000000013,5.98845674041312));
#2882=CARTESIAN_POINT('Ctrl Pts',(-46.7002923425438,1.50000000000013,5.99806873380921));
#2883=CARTESIAN_POINT('Ctrl Pts',(-46.6805980273042,1.50000000000013,6.00765136247301));
#2884=CARTESIAN_POINT('Ctrl Pts',(-46.6648305246838,1.50000000000013,6.01532332876016));
#2885=CARTESIAN_POINT('Ctrl Pts',(-46.6490504808134,1.50000000000013,6.02297484102085));
#2886=CARTESIAN_POINT('Ctrl Pts',(-46.6332652127553,1.50000000000013,6.03060245491615));
#2887=CARTESIAN_POINT('Ctrl Pts',(-46.5252097159921,1.50000000000013,6.08281605088054));
#2888=CARTESIAN_POINT('Ctrl Pts',(-46.4168069941106,1.50000000000013,6.13395988895373));
#2889=CARTESIAN_POINT('Ctrl Pts',(-46.3080494255617,1.50000000000013,6.18407421621587));
#2890=CARTESIAN_POINT('Ctrl Pts',(-46.0636310833144,1.50000000000013,6.29669958064508));
#2891=CARTESIAN_POINT('Ctrl Pts',(-45.8174223520571,1.50000000000013,6.40412874272659));
#2892=CARTESIAN_POINT('Ctrl Pts',(-45.5693210884823,1.50000000000013,6.50678841117317));
#2893=CARTESIAN_POINT('Ctrl Pts',(-45.4249966183997,1.50000000000013,6.56650718097678));
#2894=CARTESIAN_POINT('Ctrl Pts',(-45.2800312517206,1.50000000000013,6.62461106801737));
#2895=CARTESIAN_POINT('Ctrl Pts',(-45.1344011822198,1.50000000000013,6.68117694095506));
#2896=CARTESIAN_POINT('Ctrl Pts',(-44.9356631218391,1.50000000000012,6.75837110772237));
#2897=CARTESIAN_POINT('Ctrl Pts',(-44.7356876247125,1.50000000000012,6.83270186595495));
#2898=CARTESIAN_POINT('Ctrl Pts',(-44.5344076135208,1.50000000000012,6.90435191010508));
#2899=CARTESIAN_POINT('Ctrl Pts',(-44.3329812651719,1.50000000000012,6.97605404618287));
#2900=CARTESIAN_POINT('Ctrl Pts',(-44.1303200350267,1.50000000000011,7.04504802588197));
#2901=CARTESIAN_POINT('Ctrl Pts',(-43.926134663197,1.50000000000011,7.11157322203004));
#2902=CARTESIAN_POINT('Ctrl Pts',(-43.7220782177405,1.50000000000011,7.17805641295422));
#2903=CARTESIAN_POINT('Ctrl Pts',(-43.5172432493375,1.50000000000011,7.24182553985641));
#2904=CARTESIAN_POINT('Ctrl Pts',(-43.3120488965543,1.50000000000011,7.30294907653924));
#2905=CARTESIAN_POINT('Ctrl Pts',(-43.1072612505232,1.50000000000011,7.36395146293336));
#2906=CARTESIAN_POINT('Ctrl Pts',(-42.9019014984407,1.5000000000001,7.42238837429228));
#2907=CARTESIAN_POINT('Ctrl Pts',(-42.6959208043633,1.5000000000001,7.47845450070467));
#2908=CARTESIAN_POINT('Ctrl Pts',(-42.6042549864767,1.5000000000001,7.50340512705508));
#2909=CARTESIAN_POINT('Ctrl Pts',(-42.5124595070062,1.50000000000011,7.5278886704349));
#2910=CARTESIAN_POINT('Ctrl Pts',(-42.4205241992551,1.50000000000011,7.55192185945589));
#2911=CARTESIAN_POINT('Ctrl Pts',(-42.4032863290518,1.50000000000011,7.55642808239732));
#2912=CARTESIAN_POINT('Ctrl Pts',(-42.3860435428921,1.50000000000011,7.56091847155628));
#2913=CARTESIAN_POINT('Ctrl Pts',(-42.3687957735994,1.50000000000011,7.56539313583066));
#2914=CARTESIAN_POINT('Ctrl Pts',(-42.3601728119863,1.50000000000011,7.56763022850131));
#2915=CARTESIAN_POINT('Ctrl Pts',(-42.3515486048558,1.50000000000011,7.56986339078578));
#2916=CARTESIAN_POINT('Ctrl Pts',(-42.3429231438093,1.50000000000011,7.57209263625319));
#2917=CARTESIAN_POINT('Ctrl Pts',(-42.3387712046192,1.50000000000011,7.5731657025589));
#2918=CARTESIAN_POINT('Ctrl Pts',(-42.3346189748892,1.50000000000011,7.57423786131412));
#2919=CARTESIAN_POINT('Ctrl Pts',(-42.3304664536822,1.50000000000011,7.57530911403014));
#2920=CARTESIAN_POINT('Ctrl Pts',(-42.3268345793521,1.50000000000011,7.57624605210858));
#2921=CARTESIAN_POINT('Ctrl Pts',(-42.3231990849173,1.50000000000011,7.57718317460447));
#2922=CARTESIAN_POINT('Ctrl Pts',(-42.3195518619974,1.50000000000011,7.57812256321697));
#2923=CARTESIAN_POINT('Ctrl Pts',(-42.206229235501,1.50000000000011,7.60731024579269));
#2924=CARTESIAN_POINT('Ctrl Pts',(-42.0838991388229,1.50000000000011,7.63809273955698));
#2925=CARTESIAN_POINT('Ctrl Pts',(-41.9519336281348,1.50000000000011,7.67029075065104));
#2926=CARTESIAN_POINT('Ctrl Pts',(-41.8145918531791,1.50000000000011,7.70380050612157));
#2927=CARTESIAN_POINT('Ctrl Pts',(-41.6668135148127,1.50000000000011,7.73884328952492));
#2928=CARTESIAN_POINT('Ctrl Pts',(-41.5078848858298,1.50000000000011,7.77516083651302));
#2929=CARTESIAN_POINT('Ctrl Pts',(-41.4914728560587,1.50000000000011,7.77891122853614));
#2930=CARTESIAN_POINT('Ctrl Pts',(-41.4749419152315,1.50000000000011,7.78267516942519));
#2931=CARTESIAN_POINT('Ctrl Pts',(-41.4582912745849,1.50000000000011,7.78645234462284));
#2932=CARTESIAN_POINT('Ctrl Pts',(-41.2880437092141,1.50000000000011,7.82507277341156));
#2933=CARTESIAN_POINT('Ctrl Pts',(-41.105280703604,1.50000000000011,7.86508066099839));
#2934=CARTESIAN_POINT('Ctrl Pts',(-40.9091507676617,1.50000000000011,7.90609878628782));
#2935=CARTESIAN_POINT('Ctrl Pts',(-40.6940198379218,1.50000000000011,7.95109073199615));
#2936=CARTESIAN_POINT('Ctrl Pts',(-40.4628063102105,1.50000000000011,7.997296187756));
#2937=CARTESIAN_POINT('Ctrl Pts',(-40.21437984959,1.50000000000011,8.0441643485791));
#2938=CARTESIAN_POINT('Ctrl Pts',(-39.8881230599814,1.50000000000011,8.105715987027));
#2939=CARTESIAN_POINT('Ctrl Pts',(-39.5321785961021,1.50000000000011,8.16841177106708));
#2940=CARTESIAN_POINT('Ctrl Pts',(-39.1439725199136,1.50000000000011,8.23089497229237));
#2941=CARTESIAN_POINT('Ctrl Pts',(-38.9161892647587,1.50000000000011,8.2675575281888));
#2942=CARTESIAN_POINT('Ctrl Pts',(-38.6772986944323,1.50000000000011,8.30414605659786));
#2943=CARTESIAN_POINT('Ctrl Pts',(-38.4267841261925,1.50000000000011,8.34041277840537));
#2944=CARTESIAN_POINT('Ctrl Pts',(-38.1981544821903,1.50000000000011,8.37351124351358));
#2945=CARTESIAN_POINT('Ctrl Pts',(-37.9598429527006,1.50000000000011,8.40634072421756));
#2946=CARTESIAN_POINT('Ctrl Pts',(-37.7114615095564,1.50000000000011,8.43875071588523));
#2947=CARTESIAN_POINT('Ctrl Pts',(-37.4786681910349,1.50000000000011,8.46912669493609));
#2948=CARTESIAN_POINT('Ctrl Pts',(-37.2370280971275,1.50000000000011,8.4991249687636));
#2949=CARTESIAN_POINT('Ctrl Pts',(-36.9862244620814,1.50000000000011,8.52864320020706));
#2950=CARTESIAN_POINT('Ctrl Pts',(-36.8132513602342,1.50000000000011,8.54900119881773));
#2951=CARTESIAN_POINT('Ctrl Pts',(-36.6359196923416,1.50000000000011,8.56913160302865));
#2952=CARTESIAN_POINT('Ctrl Pts',(-36.454127373203,1.50000000000011,8.58901547789096));
#2953=CARTESIAN_POINT('Ctrl Pts',(-36.2135217073827,1.50000000000011,8.61533217252913));
#2954=CARTESIAN_POINT('Ctrl Pts',(-35.9651025463024,1.50000000000011,8.6412189721965));
#2955=CARTESIAN_POINT('Ctrl Pts',(-35.7086359890007,1.50000000000011,8.66665419066998));
#2956=CARTESIAN_POINT('Ctrl Pts',(-35.540534914934,1.50000000000011,8.68332571146979));
#2957=CARTESIAN_POINT('Ctrl Pts',(-35.3689766642997,1.50000000000011,8.69980407477762));
#2958=CARTESIAN_POINT('Ctrl Pts',(-35.1938969052879,1.5000000000001,8.71609544289402));
#2959=CARTESIAN_POINT('Ctrl Pts',(-34.7919055046781,1.5000000000001,8.7535011939867));
#2960=CARTESIAN_POINT('Ctrl Pts',(-34.3713714780771,1.5000000000001,8.79009866226096));
#2961=CARTESIAN_POINT('Ctrl Pts',(-33.9314440825312,1.5000000000001,8.82538571608246));
#2962=CARTESIAN_POINT('Ctrl Pts',(-33.7268155351118,1.5000000000001,8.8417991939411));
#2963=CARTESIAN_POINT('Ctrl Pts',(-33.5179894076552,1.5000000000001,8.85791559409581));
#2964=CARTESIAN_POINT('Ctrl Pts',(-33.304877686204,1.5000000000001,8.87366518630366));
#2965=CARTESIAN_POINT('Ctrl Pts',(-33.2920726363165,1.5000000000001,8.87461151770466));
#2966=CARTESIAN_POINT('Ctrl Pts',(-33.2792521138151,1.5000000000001,8.87555652343868));
#2967=CARTESIAN_POINT('Ctrl Pts',(-33.266416099541,1.5000000000001,8.87650018785329));
#2968=CARTESIAN_POINT('Ctrl Pts',(-33.257215426996,1.5000000000001,8.87717659308982));
#2969=CARTESIAN_POINT('Ctrl Pts',(-33.2480165202098,1.5000000000001,8.87785159417242));
#2970=CARTESIAN_POINT('Ctrl Pts',(-33.238819841101,1.5000000000001,8.87852515918472));
#2971=CARTESIAN_POINT('Ctrl Pts',(-33.0473126301575,1.5000000000001,8.89255115219479));
#2972=CARTESIAN_POINT('Ctrl Pts',(-32.856704989813,1.5000000000001,8.90595933266772));
#2973=CARTESIAN_POINT('Ctrl Pts',(-32.6670039177075,1.50000000000009,8.91876754736317));
#2974=CARTESIAN_POINT('Ctrl Pts',(-31.8030452793489,1.50000000000009,8.97710020518771));
#2975=CARTESIAN_POINT('Ctrl Pts',(-30.9578608360811,1.50000000000009,9.02294794423588));
#2976=CARTESIAN_POINT('Ctrl Pts',(-30.1321621754745,1.50000000000008,9.05781079611547));
#2977=CARTESIAN_POINT('Ctrl Pts',(-29.5578848243791,1.50000000000008,9.08205807564277));
#2978=CARTESIAN_POINT('Ctrl Pts',(-28.9928890954127,1.50000000000008,9.10099165420077));
#2979=CARTESIAN_POINT('Ctrl Pts',(-28.4376302401943,1.50000000000007,9.11509773780446));
#2980=CARTESIAN_POINT('Ctrl Pts',(-28.1523110222181,1.50000000000007,9.1223461350244));
#2981=CARTESIAN_POINT('Ctrl Pts',(-27.8695618760832,1.50000000000007,9.12831980439727));
#2982=CARTESIAN_POINT('Ctrl Pts',(-27.5894392714,1.50000000000007,9.13308420054702));
#2983=CARTESIAN_POINT('Ctrl Pts',(-26.9277478962211,1.50000000000006,9.14433841490715));
#2984=CARTESIAN_POINT('Ctrl Pts',(-26.281454611936,1.50000000000006,9.14884113583659));
#2985=CARTESIAN_POINT('Ctrl Pts',(-25.6506510642923,1.50000000000006,9.14749549738845));
#2986=CARTESIAN_POINT('Ctrl Pts',(-25.4470002765794,1.50000000000005,9.14706106684195));
#2987=CARTESIAN_POINT('Ctrl Pts',(-25.244964291622,1.50000000000005,9.14601684953584));
#2988=CARTESIAN_POINT('Ctrl Pts',(-25.0445471446942,1.50000000000005,9.14439258279129));
#2989=CARTESIAN_POINT('Ctrl Pts',(-24.3270447678852,1.50000000000005,9.1385776349804));
#2990=CARTESIAN_POINT('Ctrl Pts',(-23.6303730883905,1.50000000000004,9.12533114326984));
#2991=CARTESIAN_POINT('Ctrl Pts',(-22.9549224301413,1.50000000000004,9.10597228944781));
#2992=CARTESIAN_POINT('Ctrl Pts',(-22.8025170686509,1.50000000000004,9.10160425296912));
#2993=CARTESIAN_POINT('Ctrl Pts',(-22.651192098821,1.50000000000004,9.09692481967301));
#2994=CARTESIAN_POINT('Ctrl Pts',(-22.5009520119949,1.50000000000003,9.09194877207359));
#2995=CARTESIAN_POINT('Ctrl Pts',(-21.8779473032801,1.50000000000003,9.07131445835136));
#2996=CARTESIAN_POINT('Ctrl Pts',(-21.2736303287498,1.50000000000003,9.04557907659367));
#2997=CARTESIAN_POINT('Ctrl Pts',(-20.6882518298076,1.50000000000002,9.01577329099357));
#2998=CARTESIAN_POINT('Ctrl Pts',(-20.441683640011,1.50000000000002,9.00321874959145));
#2999=CARTESIAN_POINT('Ctrl Pts',(-20.1984758287443,1.50000000000002,8.98994150190267));
#3000=CARTESIAN_POINT('Ctrl Pts',(-19.9586485146901,1.50000000000002,8.97601616457639));
#3001=CARTESIAN_POINT('Ctrl Pts',(-19.5918929480637,1.50000000000002,8.95472086298948));
#3002=CARTESIAN_POINT('Ctrl Pts',(-19.2331539217403,1.50000000000001,8.93188131021674));
#3003=CARTESIAN_POINT('Ctrl Pts',(-18.8825930785396,1.50000000000001,8.90789764190378));
#3004=CARTESIAN_POINT('Ctrl Pts',(-18.8175713347727,1.50000000000001,8.90344917035916));
#3005=CARTESIAN_POINT('Ctrl Pts',(-18.7528308756026,1.50000000000001,8.89896120970124));
#3006=CARTESIAN_POINT('Ctrl Pts',(-18.6883726443041,1.50000000000001,8.89443613951083));
#3007=CARTESIAN_POINT('Ctrl Pts',(-18.3254612991177,1.50000000000001,8.86895918681165));
#3008=CARTESIAN_POINT('Ctrl Pts',(-17.9714391298583,1.50000000000001,8.84231305930845));
#3009=CARTESIAN_POINT('Ctrl Pts',(-17.6263903838312,1.50000000000001,8.81489638468738));
#3010=CARTESIAN_POINT('Ctrl Pts',(-17.5571089984659,1.50000000000001,8.80939146626143));
#3011=CARTESIAN_POINT('Ctrl Pts',(-17.4881893783597,1.50000000000001,8.80385531451122));
#3012=CARTESIAN_POINT('Ctrl Pts',(-17.4196322012764,1.50000000000001,8.79829090617308));
#3013=CARTESIAN_POINT('Ctrl Pts',(-17.0698855435987,1.5,8.76990389694932));
#3014=CARTESIAN_POINT('Ctrl Pts',(-16.7295567947277,1.5,8.74078650592042));
#3015=CARTESIAN_POINT('Ctrl Pts',(-16.3987215411361,1.5,8.71130261677436));
#3016=CARTESIAN_POINT('Ctrl Pts',(-16.1344697349496,1.5,8.68775261454312));
#3017=CARTESIAN_POINT('Ctrl Pts',(-15.8762747673998,1.5,8.66396767432586));
#3018=CARTESIAN_POINT('Ctrl Pts',(-15.6241773384801,1.5,8.64011005957217));
#3019=CARTESIAN_POINT('Ctrl Pts',(-15.4981286240202,1.5,8.62818125219533));
#3020=CARTESIAN_POINT('Ctrl Pts',(-15.3736043234866,1.5,8.61623396593671));
#3021=CARTESIAN_POINT('Ctrl Pts',(-15.2506096943136,1.5,8.60428668530748));
#3022=CARTESIAN_POINT('Ctrl Pts',(-15.1891123797271,1.5,8.59831304499287));
#3023=CARTESIAN_POINT('Ctrl Pts',(-15.1279974847049,1.5,8.59233938786278));
#3024=CARTESIAN_POINT('Ctrl Pts',(-15.0672656765957,1.5,8.5863679170989));
#3025=CARTESIAN_POINT('Ctrl Pts',(-15.0368997725411,1.5,8.58338218171695));
#3026=CARTESIAN_POINT('Ctrl Pts',(-15.0066296403192,1.5,8.58039699182383));
#3027=CARTESIAN_POINT('Ctrl Pts',(-14.9764553639702,1.5,8.57741261626164));
#3028=CARTESIAN_POINT('Ctrl Pts',(-14.9571460107395,1.5,8.57550283187321));
#3029=CARTESIAN_POINT('Ctrl Pts',(-14.9378759112039,1.5,8.57359338087164));
#3030=CARTESIAN_POINT('Ctrl Pts',(-14.9186450874746,1.5,8.57168433278082));
#3031=CARTESIAN_POINT('Ctrl Pts',(-14.907824351077,1.5,8.57061015590456));
#3032=CARTESIAN_POINT('Ctrl Pts',(-14.8970170168616,1.5,8.56953620375837));
#3033=CARTESIAN_POINT('Ctrl Pts',(-14.8862060042313,1.5,8.56846078627014));
#3034=CARTESIAN_POINT('Ctrl Pts',(-14.1315605865435,1.5,8.49339299129559));
#3035=CARTESIAN_POINT('Ctrl Pts',(-13.3783601642147,1.5,8.41312271947158));
#3036=CARTESIAN_POINT('Ctrl Pts',(-12.6255306242344,1.5,8.3290249277592));
#3037=CARTESIAN_POINT('Ctrl Pts',(-11.6940973381783,1.50000000000001,8.2249755004655));
#3038=CARTESIAN_POINT('Ctrl Pts',(-10.7632320809417,1.50000000000001,8.11506424364423));
#3039=CARTESIAN_POINT('Ctrl Pts',(-9.83090827917461,1.50000000000002,8.00182359519212));
#3040=CARTESIAN_POINT('Ctrl Pts',(-8.99377176042809,1.50000000000002,7.90014445534165));
#3041=CARTESIAN_POINT('Ctrl Pts',(-8.15545622107017,1.50000000000003,7.79578997275644));
#3042=CARTESIAN_POINT('Ctrl Pts',(-7.31449954828799,1.50000000000003,7.69052599994285));
#3043=CARTESIAN_POINT('Ctrl Pts',(-6.59897401816955,1.50000000000004,7.60096245596069));
#3044=CARTESIAN_POINT('Ctrl Pts',(-5.88153659056765,1.50000000000004,7.51073932052197));
#3045=CARTESIAN_POINT('Ctrl Pts',(-5.16128259334547,1.50000000000004,7.4209820220267));
#3046=CARTESIAN_POINT('Ctrl Pts',(-5.03502255358876,1.50000000000004,7.40524762815984));
#3047=CARTESIAN_POINT('Ctrl Pts',(-4.90867594722178,1.50000000000004,7.38952767781894));
#3048=CARTESIAN_POINT('Ctrl Pts',(-4.78223788163677,1.50000000000004,7.37382841185874));
#3049=CARTESIAN_POINT('Ctrl Pts',(-4.56955323079961,1.50000000000004,7.3474202816513));
#3050=CARTESIAN_POINT('Ctrl Pts',(-4.3566091032761,1.50000000000004,7.32107008947461));
#3051=CARTESIAN_POINT('Ctrl Pts',(-4.1433830569508,1.50000000000004,7.29480646014441));
#3052=CARTESIAN_POINT('Ctrl Pts',(-3.98346352220683,1.50000000000004,7.27510873814677));
#3053=CARTESIAN_POINT('Ctrl Pts',(-3.82338540727857,1.50000000000004,7.25545971747252));
#3054=CARTESIAN_POINT('Ctrl Pts',(-3.66313922667493,1.50000000000004,7.23587167633331));
#3055=CARTESIAN_POINT('Ctrl Pts',(-3.62715621894005,1.50000000000004,7.23147321495864));
#3056=CARTESIAN_POINT('Ctrl Pts',(-3.59116473694397,1.50000000000004,7.22707782902003));
#3057=CARTESIAN_POINT('Ctrl Pts',(-3.55516467317788,1.50000000000004,7.22268565882026));
#3058=CARTESIAN_POINT('Ctrl Pts',(-3.54355314240601,1.50000000000004,7.22126899967873));
#3059=CARTESIAN_POINT('Ctrl Pts',(-3.53194448754217,1.50000000000004,7.21985313509436));
#3060=CARTESIAN_POINT('Ctrl Pts',(-3.52034685551296,1.50000000000004,7.21843906205996));
#3061=CARTESIAN_POINT('Ctrl Pts',(-3.11130718235708,1.50000000000004,7.16856578013871));
#3062=CARTESIAN_POINT('Ctrl Pts',(-2.71295083324768,1.50000000000004,7.12055605910502));
#3063=CARTESIAN_POINT('Ctrl Pts',(-2.32483672197188,1.50000000000004,7.07445773148509));
#3064=CARTESIAN_POINT('Ctrl Pts',(-2.30225766518038,1.50000000000004,7.07177589970654));
#3065=CARTESIAN_POINT('Ctrl Pts',(-2.27971327425372,1.50000000000004,7.0691005226414));
#3066=CARTESIAN_POINT('Ctrl Pts',(-2.25720346275927,1.50000000000004,7.06643160452515));
#3067=CARTESIAN_POINT('Ctrl Pts',(-1.80960285994172,1.50000000000004,7.01336099760358));
#3068=CARTESIAN_POINT('Ctrl Pts',(-1.37567372863184,1.50000000000004,6.96285895545701));
#3069=CARTESIAN_POINT('Ctrl Pts',(-0.954738519600669,1.50000000000004,6.9148961501584));
#3070=CARTESIAN_POINT('Ctrl Pts',(-0.533803310569499,1.50000000000004,6.86693334485979));
#3071=CARTESIAN_POINT('Ctrl Pts',(-0.125862135491728,1.50000000000004,6.82150863908376));
#3072=CARTESIAN_POINT('Ctrl Pts',(0.269757237238929,1.50000000000004,6.77853867313061));
#3073=CARTESIAN_POINT('Ctrl Pts',(0.705941810521693,1.50000000000004,6.73116274172998));
#3074=CARTESIAN_POINT('Ctrl Pts',(1.12715344954864,1.50000000000004,6.68682581445775));
#3075=CARTESIAN_POINT('Ctrl Pts',(1.53428028329925,1.50000000000004,6.64528629088636));
#3076=CARTESIAN_POINT('Ctrl Pts',(1.87215098302727,1.50000000000004,6.61081303407316));
#3077=CARTESIAN_POINT('Ctrl Pts',(2.2003275842666,1.50000000000004,6.57833169383247));
#3078=CARTESIAN_POINT('Ctrl Pts',(2.51930177206597,1.50000000000004,6.54754073376113));
#3079=CARTESIAN_POINT('Ctrl Pts',(2.61354920273931,1.50000000000004,6.53844291649037));
#3080=CARTESIAN_POINT('Ctrl Pts',(2.70699327148389,1.50000000000004,6.5294930242348));
#3081=CARTESIAN_POINT('Ctrl Pts',(2.79964674389792,1.50000000000004,6.52068412397982));
#3082=CARTESIAN_POINT('Ctrl Pts',(3.10485723459384,1.50000000000003,6.49166666031369));
#3083=CARTESIAN_POINT('Ctrl Pts',(3.40148201654041,1.50000000000003,6.46410905983882));
#3084=CARTESIAN_POINT('Ctrl Pts',(3.68997607232203,1.50000000000003,6.43774996449062));
#3085=CARTESIAN_POINT('Ctrl Pts',(3.99784226211859,1.50000000000003,6.40962087798535));
#3086=CARTESIAN_POINT('Ctrl Pts',(4.29644914071748,1.50000000000003,6.38285685673465));
#3087=CARTESIAN_POINT('Ctrl Pts',(4.58635565562216,1.50000000000003,6.35720199708492));
#3088=CARTESIAN_POINT('Ctrl Pts',(4.84164454089151,1.50000000000003,6.33461057472978));
#3089=CARTESIAN_POINT('Ctrl Pts',(5.09018694388211,1.50000000000003,6.31288049665803));
#3090=CARTESIAN_POINT('Ctrl Pts',(5.33236776508438,1.50000000000003,6.29187011097832));
#3091=CARTESIAN_POINT('Ctrl Pts',(5.6345644513341,1.50000000000003,6.26565305176728));
#3092=CARTESIAN_POINT('Ctrl Pts',(5.92685513364938,1.50000000000003,6.24054875616991));
#3093=CARTESIAN_POINT('Ctrl Pts',(6.20999223681358,1.50000000000003,6.21632922031447));
#3094=CARTESIAN_POINT('Ctrl Pts',(6.52078059810494,1.50000000000002,6.18974439700579));
#3095=CARTESIAN_POINT('Ctrl Pts',(6.82054022294184,1.50000000000002,6.16422587194136));
#3096=CARTESIAN_POINT('Ctrl Pts',(7.11027273672712,1.50000000000002,6.13953902411822));
#3097=CARTESIAN_POINT('Ctrl Pts',(7.37008754579113,1.50000000000002,6.11740133384052));
#3098=CARTESIAN_POINT('Ctrl Pts',(7.62183926725666,1.50000000000002,6.09593391271264));
#3099=CARTESIAN_POINT('Ctrl Pts',(7.86625360733992,1.50000000000002,6.07500271807589));
#3100=CARTESIAN_POINT('Ctrl Pts',(8.09291279008128,1.50000000000002,6.05559204246434));
#3101=CARTESIAN_POINT('Ctrl Pts',(8.31326296260427,1.50000000000002,6.03664426550279));
#3102=CARTESIAN_POINT('Ctrl Pts',(8.52788366706357,1.50000000000002,6.01806828389815));
#3103=CARTESIAN_POINT('Ctrl Pts',(8.68884919540805,1.50000000000002,6.00413629769468));
#3104=CARTESIAN_POINT('Ctrl Pts',(8.84659194283416,1.50000000000002,5.99041384636439));
#3105=CARTESIAN_POINT('Ctrl Pts',(9.00135696938046,1.50000000000002,5.9768675024729));
#3106=CARTESIAN_POINT('Ctrl Pts',(9.01581102489525,1.50000000000002,5.97560236130374));
#3107=CARTESIAN_POINT('Ctrl Pts',(9.03023910795808,1.50000000000002,5.97433875874388));
#3108=CARTESIAN_POINT('Ctrl Pts',(9.04464141836935,1.50000000000002,5.97307666907199));
#3109=CARTESIAN_POINT('Ctrl Pts',(9.05358082167618,1.50000000000002,5.97229329971913));
#3110=CARTESIAN_POINT('Ctrl Pts',(9.06250938704645,1.50000000000002,5.97151059322107));
#3111=CARTESIAN_POINT('Ctrl Pts',(9.07144369583731,1.50000000000002,5.97072709265066));
#3112=CARTESIAN_POINT('Ctrl Pts',(9.51048454911024,1.50000000000002,5.93222509243753));
#3113=CARTESIAN_POINT('Ctrl Pts',(9.95403537666102,1.50000000000002,5.8926258316374));
#3114=CARTESIAN_POINT('Ctrl Pts',(10.3995073164968,1.50000000000002,5.85165205131927));
#3115=CARTESIAN_POINT('Ctrl Pts',(10.8207555645272,1.50000000000002,5.81290632654801));
#3116=CARTESIAN_POINT('Ctrl Pts',(11.2437548001683,1.50000000000002,5.77293047513436));
#3117=CARTESIAN_POINT('Ctrl Pts',(11.6662637360807,1.50000000000002,5.73147701131878));
#3118=CARTESIAN_POINT('Ctrl Pts',(12.0374006682032,1.50000000000002,5.69506379001463));
#3119=CARTESIAN_POINT('Ctrl Pts',(12.4081589691877,1.50000000000001,5.65750947828726));
#3120=CARTESIAN_POINT('Ctrl Pts',(12.7770243679439,1.50000000000001,5.61868654953851));
#3121=CARTESIAN_POINT('Ctrl Pts',(12.8280819508003,1.50000000000001,5.61331276032435));
#3122=CARTESIAN_POINT('Ctrl Pts',(12.8791032787792,1.50000000000001,5.60791474655984));
#3123=CARTESIAN_POINT('Ctrl Pts',(12.9300843489308,1.50000000000001,5.60249225367133));
#3124=CARTESIAN_POINT('Ctrl Pts',(13.2595479279469,1.50000000000001,5.56744956216012));
#3125=CARTESIAN_POINT('Ctrl Pts',(13.5873394667212,1.50000000000001,5.53138422159486));
#3126=CARTESIAN_POINT('Ctrl Pts',(13.9123956890807,1.50000000000001,5.49422080575756));
#3127=CARTESIAN_POINT('Ctrl Pts',(14.2186795743761,1.50000000000001,5.45920361608227));
#3128=CARTESIAN_POINT('Ctrl Pts',(14.5225349237245,1.50000000000001,5.42321129865508));
#3129=CARTESIAN_POINT('Ctrl Pts',(14.8230783860206,1.50000000000001,5.38622616438368));
#3130=CARTESIAN_POINT('Ctrl Pts',(15.035316648525,1.50000000000001,5.36010794315775));
#3131=CARTESIAN_POINT('Ctrl Pts',(15.2459034227506,1.50000000000001,5.33349553417475));
#3132=CARTESIAN_POINT('Ctrl Pts',(15.454529747749,1.50000000000001,5.30639838000327));
#3133=CARTESIAN_POINT('Ctrl Pts',(15.7314585932908,1.50000000000001,5.27042984332779));
#3134=CARTESIAN_POINT('Ctrl Pts',(16.0049330589367,1.50000000000001,5.23360279460352));
#3135=CARTESIAN_POINT('Ctrl Pts',(16.2742336283039,1.5,5.19595898559869));
#3136=CARTESIAN_POINT('Ctrl Pts',(16.4219131180616,1.5,5.17531581161865));
#3137=CARTESIAN_POINT('Ctrl Pts',(16.5683375408946,1.5,5.15442789297188));
#3138=CARTESIAN_POINT('Ctrl Pts',(16.7133891339298,1.5,5.13330876447839));
#3139=CARTESIAN_POINT('Ctrl Pts',(16.9684975087711,1.5,5.09616565949551));
#3140=CARTESIAN_POINT('Ctrl Pts',(17.2193592251396,1.5,5.05830547382683));
#3141=CARTESIAN_POINT('Ctrl Pts',(17.4653369451222,1.5,5.01982643614904));
#3142=CARTESIAN_POINT('Ctrl Pts',(17.635772215158,1.5,4.9931647320817));
#3143=CARTESIAN_POINT('Ctrl Pts',(17.8038628427899,1.5,4.96620697017877));
#3144=CARTESIAN_POINT('Ctrl Pts',(17.9693987744903,1.5,4.93900041044443));
#3145=CARTESIAN_POINT('Ctrl Pts',(18.1827156839134,1.5,4.90394083649605));
#3146=CARTESIAN_POINT('Ctrl Pts',(18.3917899704582,1.5,4.86846598332765));
#3147=CARTESIAN_POINT('Ctrl Pts',(18.5961751592073,1.5,4.83269950369486));
#3148=CARTESIAN_POINT('Ctrl Pts',(18.7017980573384,1.5,4.81421597630288));
#3149=CARTESIAN_POINT('Ctrl Pts',(18.806168729909,1.5,4.7956550811478));
#3150=CARTESIAN_POINT('Ctrl Pts',(18.9092259812001,1.5,4.77703704590836));
#3151=CARTESIAN_POINT('Ctrl Pts',(19.0149000522275,1.5,4.7579462633226));
#3152=CARTESIAN_POINT('Ctrl Pts',(19.1191939813236,1.5,4.73879804741868));
#3153=CARTESIAN_POINT('Ctrl Pts',(19.2220396298678,1.5,4.71960863557561));
#3154=CARTESIAN_POINT('Ctrl Pts',(19.3277806393804,1.5,4.69987899403062));
#3155=CARTESIAN_POINT('Ctrl Pts',(19.4319522489605,1.5,4.68014548934906));
#3156=CARTESIAN_POINT('Ctrl Pts',(19.5344534591269,1.5,4.66032590026468));
#3157=CARTESIAN_POINT('Ctrl Pts',(19.6401702303914,1.5,4.63988455169533));
#3158=CARTESIAN_POINT('Ctrl Pts',(19.7441057609561,1.5,4.61933682528627));
#3159=CARTESIAN_POINT('Ctrl Pts',(19.8461483400865,1.5,4.5985899959703));
#3160=CARTESIAN_POINT('Ctrl Pts',(19.9603425121877,1.5,4.57537256048748));
#3161=CARTESIAN_POINT('Ctrl Pts',(20.0721640111897,1.5,4.55189882105127));
#3162=CARTESIAN_POINT('Ctrl Pts',(20.1814687083029,1.5,4.52808124461801));
#3163=CARTESIAN_POINT('Ctrl Pts',(20.2784032176319,1.5,4.50695914148847));
#3164=CARTESIAN_POINT('Ctrl Pts',(20.3733585787686,1.5,4.48556739870102));
#3165=CARTESIAN_POINT('Ctrl Pts',(20.466243911377,1.5,4.46387787110044));
#3166=CARTESIAN_POINT('Ctrl Pts',(20.5763630626326,1.5,4.43816409796275));
#3167=CARTESIAN_POINT('Ctrl Pts',(20.6835711433518,1.5,4.41202618656764));
#3168=CARTESIAN_POINT('Ctrl Pts',(20.7877374720262,1.5,4.38548804258589));
#3169=CARTESIAN_POINT('Ctrl Pts',(20.8880371211572,1.5,4.3599350009857));
#3170=CARTESIAN_POINT('Ctrl Pts',(20.9855167974935,1.5,4.33401139842294));
#3171=CARTESIAN_POINT('Ctrl Pts',(21.0800726838929,1.5,4.30778240560577));
#3172=CARTESIAN_POINT('Ctrl Pts',(21.1899754169482,1.5,4.27729632900427));
#3173=CARTESIAN_POINT('Ctrl Pts',(21.2959271796799,1.5,4.24639403035665));
#3174=CARTESIAN_POINT('Ctrl Pts',(21.3977943899266,1.5,4.21527827297281));
#3175=CARTESIAN_POINT('Ctrl Pts',(21.4546405350168,1.5,4.19791438468579));
#3176=CARTESIAN_POINT('Ctrl Pts',(21.5102149898772,1.5,4.1804849859871));
#3177=CARTESIAN_POINT('Ctrl Pts',(21.5644964972823,1.5,4.16303198962476));
#3178=CARTESIAN_POINT('',(21.3356435067856,1.5,3.73655812712738));
#3179=CARTESIAN_POINT('',(22.5271211105952,1.5,5.95690952216869));
#3180=CARTESIAN_POINT('',(21.3356435067856,1.5,3.73655812712738));
#3181=CARTESIAN_POINT('Origin',(1.90003279625137,0.,8.11589060443533));
#3182=CARTESIAN_POINT('',(21.3356435067856,0.,3.73655812712738));
#3183=CARTESIAN_POINT('',(21.3356435067856,0.,3.73655812712738));
#3184=CARTESIAN_POINT('',(22.284188719917,-3.50719883690508E-10,5.50419830755606));
#3185=CARTESIAN_POINT('',(22.5271211105952,0.,5.95690952216869));
#3186=CARTESIAN_POINT('Ctrl Pts',(-51.6806944441105,-1.50990331349021E-14,
4.46173484851326));
#3187=CARTESIAN_POINT('Ctrl Pts',(-51.6763944115022,5.87692512758708E-13,
4.46557237996829));
#3188=CARTESIAN_POINT('Ctrl Pts',(-51.6717236003112,-1.02756276505808E-14,
4.46973835626723));
#3189=CARTESIAN_POINT('Ctrl Pts',(-51.6618445772489,-1.26565424807279E-14,
4.47853832467601));
#3190=CARTESIAN_POINT('Ctrl Pts',(-51.6562942458247,-1.36557432028894E-14,
4.48347711152442));
#3191=CARTESIAN_POINT('Ctrl Pts',(-51.6399305987615,-1.54321000422896E-14,
4.49801845622271));
#3192=CARTESIAN_POINT('Ctrl Pts',(-51.6289127938884,-1.63757896132209E-14,
4.50778632959587));
#3193=CARTESIAN_POINT('Ctrl Pts',(-51.6069503571003,-1.63757896132212E-14,
4.52720927807316));
#3194=CARTESIAN_POINT('Ctrl Pts',(-51.5959572964355,-1.54321000422898E-14,
4.53690769597779));
#3195=CARTESIAN_POINT('Ctrl Pts',(-51.5629426093583,-9.71445146546972E-15,
4.56596373819379));
#3196=CARTESIAN_POINT('Ctrl Pts',(-51.5188283460193,-1.97064586869581E-14,
4.60460056353571));
#3197=CARTESIAN_POINT('Ctrl Pts',(-51.4745249624866,-1.48214773787458E-14,
4.64302781421577));
#3198=CARTESIAN_POINT('Ctrl Pts',(-51.4079282366868,-5.60662627435695E-15,
4.70051118190272));
#3199=CARTESIAN_POINT('Ctrl Pts',(-51.3633415497112,-1.40998324127395E-14,
4.73862341351609));
#3200=CARTESIAN_POINT('Ctrl Pts',(-51.229016501315,-9.99200722162641E-15,
4.85232753950401));
#3201=CARTESIAN_POINT('Ctrl Pts',(-51.13870277151,-1.55431223447521E-14,
4.92729489364781));
#3202=CARTESIAN_POINT('Ctrl Pts',(-50.956619740663,-1.47104550762833E-14,
5.0754979207133));
#3203=CARTESIAN_POINT('Ctrl Pts',(-50.8647490823044,-1.55431223447522E-14,
5.14881255305296));
#3204=CARTESIAN_POINT('Ctrl Pts',(-50.6798803771769,-1.47104550762833E-14,
5.29345224746616));
#3205=CARTESIAN_POINT('Ctrl Pts',(-50.5869566911128,-1.51545442861334E-14,
5.36472658268942));
#3206=CARTESIAN_POINT('Ctrl Pts',(-50.1197141929288,-9.82547376793259E-15,
5.71605324160813));
#3207=CARTESIAN_POINT('Ctrl Pts',(-49.7378902077951,-1.52655665885959E-14,
5.98082374985693));
#3208=CARTESIAN_POINT('Ctrl Pts',(-48.9598663397128,-1.52655665885959E-14,
6.47927805260146));
#3209=CARTESIAN_POINT('Ctrl Pts',(-48.5636892956867,-1.52655665885959E-14,
6.71296610783997));
#3210=CARTESIAN_POINT('Ctrl Pts',(-47.7587593461934,-1.52655665885959E-14,
7.15109273394721));
#3211=CARTESIAN_POINT('Ctrl Pts',(-47.3500098510032,-1.47104550762833E-14,
7.3555359494196));
#3212=CARTESIAN_POINT('Ctrl Pts',(-46.5215810175673,-1.55431223447522E-14,
7.73726655172034));
#3213=CARTESIAN_POINT('Ctrl Pts',(-46.1019027012514,-1.46549439250521E-14,
7.91455864407753));
#3214=CARTESIAN_POINT('Ctrl Pts',(-45.4653032959013,-1.32116539930394E-14,
8.16182742932691));
#3215=CARTESIAN_POINT('Ctrl Pts',(-45.251921935563,-1.07136521876328E-14,
8.24114014723876));
#3216=CARTESIAN_POINT('Ctrl Pts',(-44.8229670778109,-1.23234755733392E-14,
8.39383604775355));
#3217=CARTESIAN_POINT('Ctrl Pts',(-44.6074695243589,-1.43218770176645E-14,
8.46719451744161));
#3218=CARTESIAN_POINT('Ctrl Pts',(-44.1741403300322,-1.2490009027033E-14,
8.60837654140212));
#3219=CARTESIAN_POINT('Ctrl Pts',(-43.957100425155,-9.88098491916389E-15,
8.67593604627367));
#3220=CARTESIAN_POINT('Ctrl Pts',(-43.5234563762582,-1.10467190950203E-14,
8.80511044508152));
#3221=CARTESIAN_POINT('Ctrl Pts',(-43.3066239379348,-1.48214773787458E-14,
8.86679975726875));
#3222=CARTESIAN_POINT('Ctrl Pts',(-42.6563779943798,-1.53210777398272E-14,
9.04379102211169));
#3223=CARTESIAN_POINT('Ctrl Pts',(-42.2230732679144,-1.52655665885959E-14,
9.15107362497687));
#3224=CARTESIAN_POINT('Ctrl Pts',(-41.3571906888076,-1.52655665885959E-14,
9.34749799494818));
#3225=CARTESIAN_POINT('Ctrl Pts',(-40.9245970789775,-1.53210777398272E-14,
9.43663506835774));
#3226=CARTESIAN_POINT('Ctrl Pts',(-39.6281635689816,-1.39332989590457E-14,
9.68122246026781));
#3227=CARTESIAN_POINT('Ctrl Pts',(-38.7656553292243,-1.33226762955019E-14,
9.81390977310064));
#3228=CARTESIAN_POINT('Ctrl Pts',(-37.4754796214115,-1.33226762955019E-14,
9.98225882431641));
#3229=CARTESIAN_POINT('Ctrl Pts',(-37.0460144673576,-1.47104550762833E-14,
10.0332224910664));
#3230=CARTESIAN_POINT('Ctrl Pts',(-36.188424525307,-1.52655665885959E-14,
10.1270230508065));
#3231=CARTESIAN_POINT('Ctrl Pts',(-35.7602421886007,-1.49880108324396E-14,
10.1698763527029));
#3232=CARTESIAN_POINT('Ctrl Pts',(-34.9056083623748,-1.51545442861334E-14,
10.2494008139146));
#3233=CARTESIAN_POINT('Ctrl Pts',(-34.4788493666452,-1.52655665885959E-14,
10.2862947402486));
#3234=CARTESIAN_POINT('Ctrl Pts',(-33.6238677315729,-1.52655665885959E-14,
10.3548750069945));
#3235=CARTESIAN_POINT('Ctrl Pts',(-33.1961718222826,-1.52655665885959E-14,
10.3864537666074));
#3236=CARTESIAN_POINT('Ctrl Pts',(-31.9117882640685,-1.55431223447522E-14,
10.4731744098343));
#3237=CARTESIAN_POINT('Ctrl Pts',(-31.0542758170156,-1.51545442861334E-14,
10.5202135306195));
#3238=CARTESIAN_POINT('Ctrl Pts',(-29.3366002909415,-1.4432899320127E-14,
10.5927376485604));
#3239=CARTESIAN_POINT('Ctrl Pts',(-28.4761608671941,-1.49880108324396E-14,
10.6182195605205));
#3240=CARTESIAN_POINT('Ctrl Pts',(-26.7537363343169,-1.49880108324396E-14,
10.6475149919468));
#3241=CARTESIAN_POINT('Ctrl Pts',(-25.8929997326651,-1.50990331349021E-14,
10.6513180682083));
#3242=CARTESIAN_POINT('Ctrl Pts',(-24.1717820662198,-1.52655665885959E-14,
10.6373685795577));
#3243=CARTESIAN_POINT('Ctrl Pts',(-23.3114174177265,-1.55431223447522E-14,
10.619614411021));
#3244=CARTESIAN_POINT('Ctrl Pts',(-21.5911791490513,-1.47104550762833E-14,
10.5626390207657));
#3245=CARTESIAN_POINT('Ctrl Pts',(-20.7314512337837,-1.45439216225896E-14,
10.5234146492955));
#3246=CARTESIAN_POINT('Ctrl Pts',(-19.4417924804905,-1.52655665885959E-14,
10.4485318669319));
#3247=CARTESIAN_POINT('Ctrl Pts',(-19.0122168333525,-1.53210777398272E-14,
10.4208622983205));
#3248=CARTESIAN_POINT('Ctrl Pts',(-18.1544474369902,-1.28785870856518E-14,
10.3606452684977));
#3249=CARTESIAN_POINT('Ctrl Pts',(-17.7260787333555,-9.6034291630076E-15,
10.3280962329425));
#3250=CARTESIAN_POINT('Ctrl Pts',(-16.4427007962872,-1.16018306073329E-14,
10.2239312028492));
#3251=CARTESIAN_POINT('Ctrl Pts',(-15.5892294662238,-1.52655665885959E-14,
10.1457967780066));
#3252=CARTESIAN_POINT('Ctrl Pts',(-13.0347334107054,-1.47104550762833E-14,
9.89168964726816));
#3253=CARTESIAN_POINT('Ctrl Pts',(-11.3394546576359,-1.53210777398272E-14,
9.69607640520465));
#3254=CARTESIAN_POINT('Ctrl Pts',(-7.96064496793785,-1.46549439250521E-14,
9.28568442648744));
#3255=CARTESIAN_POINT('Ctrl Pts',(-6.27708213802847,-1.33781874467331E-14,
9.07095521078264));
#3256=CARTESIAN_POINT('Ctrl Pts',(-3.75757592845614,-1.40443212615082E-14,
8.75811925740311));
#3257=CARTESIAN_POINT('Ctrl Pts',(-2.91870135734488,-1.49880108324396E-14,
8.65537011020776));
#3258=CARTESIAN_POINT('Ctrl Pts',(-1.24247939398972,-1.53210777398272E-14,
8.456625736016));
#3259=CARTESIAN_POINT('Ctrl Pts',(-0.40523588459794,-1.55431223447522E-14,
8.36067304622072));
#3260=CARTESIAN_POINT('Ctrl Pts',(0.850126830267879,-1.52655665885959E-14,
8.22432478760327));
#3261=CARTESIAN_POINT('Ctrl Pts',(1.26837589519449,-1.46549439250521E-14,
8.18020417904461));
#3262=CARTESIAN_POINT('Ctrl Pts',(2.10462556977151,-1.53210777398272E-14,
8.09488104961065));
#3263=CARTESIAN_POINT('Ctrl Pts',(2.52277657874592,-1.52655665885959E-14,
8.05377185277432));
#3264=CARTESIAN_POINT('Ctrl Pts',(3.77964787852141,-1.47104550762833E-14,
7.9342744779821));
#3265=CARTESIAN_POINT('Ctrl Pts',(4.61982937965303,-1.49880108324396E-14,
7.85932056880712));
#3266=CARTESIAN_POINT('Ctrl Pts',(6.30419335006199,-1.53210777398272E-14,
7.71319367407381));
#3267=CARTESIAN_POINT('Ctrl Pts',(7.14835445371892,-1.53210777398272E-14,
7.64197271158988));
#3268=CARTESIAN_POINT('Ctrl Pts',(8.84012615676403,-1.49324996812084E-14,
7.49709237947704));
#3269=CARTESIAN_POINT('Ctrl Pts',(9.68774962954449,-1.52655665885959E-14,
7.42345015929489));
#3270=CARTESIAN_POINT('Ctrl Pts',(11.3860360205753,-1.50990331349021E-14,
7.2672442573381));
#3271=CARTESIAN_POINT('Ctrl Pts',(12.2368316890249,-1.51545442861334E-14,
7.18468982285689));
#3272=CARTESIAN_POINT('Ctrl Pts',(13.9406285449295,-1.49880108324396E-14,
7.0034685113226));
#3273=CARTESIAN_POINT('Ctrl Pts',(14.7936901482575,-1.53210777398272E-14,
6.90483054595407));
#3274=CARTESIAN_POINT('Ctrl Pts',(16.0747466690875,-1.48214773787458E-14,
6.73844149943281));
#3275=CARTESIAN_POINT('Ctrl Pts',(16.50201152176,-1.51545442861334E-14,
6.67990037484624));
#3276=CARTESIAN_POINT('Ctrl Pts',(17.3570006606566,-1.49880108324396E-14,
6.5554161693539));
#3277=CARTESIAN_POINT('Ctrl Pts',(17.7847249958247,-1.47104550762833E-14,
6.48947667417001));
#3278=CARTESIAN_POINT('Ctrl Pts',(18.4266366353337,-1.52655665885959E-14,
6.38397561990512));
#3279=CARTESIAN_POINT('Ctrl Pts',(18.6406614273411,-1.55431223447522E-14,
6.34770897366403));
#3280=CARTESIAN_POINT('Ctrl Pts',(18.9617779205806,-1.52655665885959E-14,
6.29151504371349));
#3281=CARTESIAN_POINT('Ctrl Pts',(19.068829972339,-1.55986334959835E-14,
6.27248467831306));
#3282=CARTESIAN_POINT('Ctrl Pts',(19.2829601978757,-1.42663658664332E-14,
6.23380050962898));
#3283=CARTESIAN_POINT('Ctrl Pts',(19.3900589556033,-1.50990331349021E-14,
6.21414596127395));
#3284=CARTESIAN_POINT('Ctrl Pts',(19.6041999526691,-1.51545442861334E-14,
6.17419022140595));
#3285=CARTESIAN_POINT('Ctrl Pts',(19.7112453138705,-1.52655665885959E-14,
6.1539249037101));
#3286=CARTESIAN_POINT('Ctrl Pts',(19.927225613168,-1.52655665885959E-14,
6.11216350959792));
#3287=CARTESIAN_POINT('Ctrl Pts',(20.0357720315265,-1.52655665885959E-14,
6.09072507683146));
#3288=CARTESIAN_POINT('Ctrl Pts',(20.3635135134148,-1.52655665885959E-14,
6.02409147505319));
#3289=CARTESIAN_POINT('Ctrl Pts',(20.5844252421794,-1.49880108324396E-14,
5.97663273062336));
#3290=CARTESIAN_POINT('Ctrl Pts',(21.0302529664136,-1.51545442861334E-14,
5.87252956963633));
#3291=CARTESIAN_POINT('Ctrl Pts',(21.255123956843,-1.52655665885959E-14,
5.8158636933129));
#3292=CARTESIAN_POINT('Ctrl Pts',(21.7069290696632,-1.52655665885959E-14,
5.69053907719101));
#3293=CARTESIAN_POINT('Ctrl Pts',(21.9338427022935,-1.52655665885959E-14,
5.62185435786818));
#3294=CARTESIAN_POINT('Ctrl Pts',(22.2017782898667,-1.52655665885959E-14,
5.53241479386655));
#3295=CARTESIAN_POINT('Ctrl Pts',(22.2429910739314,-1.52655665885959E-14,
5.51842350402865));
#3296=CARTESIAN_POINT('Ctrl Pts',(22.2841887200099,-1.50990331349021E-14,
5.50419830661928));
#3297=CARTESIAN_POINT('Origin',(22.5271211105952,0.,5.95690952216869));
#3298=CARTESIAN_POINT('Ctrl Pts',(21.5644964972421,1.49999999933821,4.16303199033283));
#3299=CARTESIAN_POINT('Ctrl Pts',(21.681228802004,1.25717622640274,4.38056586163327));
#3300=CARTESIAN_POINT('Ctrl Pts',(21.7980931140595,1.01382299981494,4.59834573216322));
#3301=CARTESIAN_POINT('Ctrl Pts',(22.0379173769264,0.513975656786509,5.0452648642717));
#3302=CARTESIAN_POINT('Ctrl Pts',(22.1612401129227,0.256699533297706,5.27508018605377));
#3303=CARTESIAN_POINT('Ctrl Pts',(22.2841887197601,-1.05214455203839E-9,
5.50419830781864));
#3304=CARTESIAN_POINT('',(21.3356435067856,0.,3.73655812712738));
#3305=CARTESIAN_POINT('Origin',(21.3356435067856,0.,3.73655812712738));
#3306=CARTESIAN_POINT('Ctrl Pts',(-53.4855959126572,1.50000424468862,0.840085176636737));
#3307=CARTESIAN_POINT('Ctrl Pts',(-53.1643320247582,1.50000424468862,1.1268400488604));
#3308=CARTESIAN_POINT('Ctrl Pts',(-52.8430681368593,1.50000424468862,1.41359492108406));
#3309=CARTESIAN_POINT('Ctrl Pts',(-52.3611723050108,1.50000424468862,1.84372722941957));
#3310=CARTESIAN_POINT('Ctrl Pts',(-52.2005403610613,1.50000424468862,1.98710466553139));
#3311=CARTESIAN_POINT('Ctrl Pts',(-51.8792764731623,1.50000424468862,2.27385953775507));
#3312=CARTESIAN_POINT('Ctrl Pts',(-51.7186445292128,1.50000424468862,2.41723697386691));
#3313=CARTESIAN_POINT('Ctrl Pts',(-51.4776966132886,1.50000424468862,2.63230312803465));
#3314=CARTESIAN_POINT('Ctrl Pts',(-51.3973806413139,1.50000424468862,2.70399184609058));
#3315=CARTESIAN_POINT('Ctrl Pts',(-51.2367486973644,1.50000424468862,2.84736928220241));
#3316=CARTESIAN_POINT('Ctrl Pts',(-51.1564327253896,1.50000424468862,2.91905800025832));
#3317=CARTESIAN_POINT('Ctrl Pts',(-50.9958007814402,1.50000424468862,3.06243543637014));
#3318=CARTESIAN_POINT('Ctrl Pts',(-50.9155056164988,1.50000424468862,3.13414750105302));
#3319=CARTESIAN_POINT('Ctrl Pts',(-50.8150846427386,1.50000424468862,3.22372921533924));
#3320=CARTESIAN_POINT('Ctrl Pts',(-50.7950108515033,1.50000424468862,3.24165723150992));
#3321=CARTESIAN_POINT('Ctrl Pts',(-50.7648923620128,1.50000424468862,3.26854050078091));
#3322=CARTESIAN_POINT('Ctrl Pts',(-50.7548528655159,1.50000424468862,3.2775015905379));
#3323=CARTESIAN_POINT('Ctrl Pts',(-50.7347738725222,1.50000424468862,3.29542377005189));
#3324=CARTESIAN_POINT('Ctrl Pts',(-50.7247343760254,1.50000424468862,3.30438485980889));
#3325=CARTESIAN_POINT('Ctrl Pts',(-50.7096751312801,1.50000424468862,3.31782649444435));
#3326=CARTESIAN_POINT('Ctrl Pts',(-50.7046553830317,1.50000424468862,3.32230703932284));
#3327=CARTESIAN_POINT('Ctrl Pts',(-50.6946158865349,1.50000424468862,3.33126812907983));
#3328=CARTESIAN_POINT('Ctrl Pts',(-50.6895959364334,1.50000424468862,3.33574844718509));
#3329=CARTESIAN_POINT('Ctrl Pts',(-50.6795568436426,1.50000424468862,3.34470999048859));
#3330=CARTESIAN_POINT('Ctrl Pts',(-50.6745359674055,1.50000424468862,3.34918926458991));
#3331=CARTESIAN_POINT('Ctrl Pts',(-50.6644875302798,1.50000424468862,3.35814031000442));
#3332=CARTESIAN_POINT('Ctrl Pts',(-50.6594607930231,1.50000424468862,3.36261300364892));
#3333=CARTESIAN_POINT('Ctrl Pts',(-50.6443721387661,1.50000424468862,3.37602160585764));
#3334=CARTESIAN_POINT('Ctrl Pts',(-50.6343023847501,1.50000424468862,3.38494871278844));
#3335=CARTESIAN_POINT('Ctrl Pts',(-50.6141412499045,1.50000424468862,3.40277864154937));
#3336=CARTESIAN_POINT('Ctrl Pts',(-50.60404992209,1.50000424468862,3.41168152263516));
#3337=CARTESIAN_POINT('Ctrl Pts',(-50.5737436481473,1.50000424468863,3.43835390553867));
#3338=CARTESIAN_POINT('Ctrl Pts',(-50.5534964114456,1.50000424468862,3.45608714691913));
#3339=CARTESIAN_POINT('Ctrl Pts',(-50.5129157820777,1.50000424468862,3.49145688153963));
#3340=CARTESIAN_POINT('Ctrl Pts',(-50.4925823894169,1.50000424468862,3.50909337478607));
#3341=CARTESIAN_POINT('Ctrl Pts',(-50.4314529095512,1.50000424468862,3.56185765602773));
#3342=CARTESIAN_POINT('Ctrl Pts',(-50.3905275193144,1.50000424468862,3.59684024423588));
#3343=CARTESIAN_POINT('Ctrl Pts',(-50.2672336401988,1.50000424468862,3.70120665243317));
#3344=CARTESIAN_POINT('Ctrl Pts',(-50.1843379300463,1.50000424468862,3.77001650401763));
#3345=CARTESIAN_POINT('Ctrl Pts',(-50.0172017432821,1.50000424468862,3.90605383105355));
#3346=CARTESIAN_POINT('Ctrl Pts',(-49.9328682048228,1.50000424468862,3.97335380373027));
#3347=CARTESIAN_POINT('Ctrl Pts',(-49.7631459041653,1.50000424468862,4.10614308134383));
#3348=CARTESIAN_POINT('Ctrl Pts',(-49.677825339688,1.50000424468862,4.1715858145101));
#3349=CARTESIAN_POINT('Ctrl Pts',(-49.2487341885864,1.50000424468862,4.49422615931033));
#3350=CARTESIAN_POINT('Ctrl Pts',(-48.8978315305851,1.50000424468862,4.73757809459553));
#3351=CARTESIAN_POINT('Ctrl Pts',(-48.1815619571434,1.50000424468862,5.19646908789177));
#3352=CARTESIAN_POINT('Ctrl Pts',(-47.8162114076662,1.50000424468862,5.41201043441217));
#3353=CARTESIAN_POINT('Ctrl Pts',(-47.0720114983415,1.50000424468862,5.81708209356818));
#3354=CARTESIAN_POINT('Ctrl Pts',(-46.6931626858749,1.50000424468862,6.00661346095856));
#3355=CARTESIAN_POINT('Ctrl Pts',(-45.9229326124668,1.50000424468862,6.361527261268));
#3356=CARTESIAN_POINT('Ctrl Pts',(-45.5315517688313,1.50000424468862,6.52691049828853));
#3357=CARTESIAN_POINT('Ctrl Pts',(-44.9358235836156,1.50000424468862,6.7583042272479));
#3358=CARTESIAN_POINT('Ctrl Pts',(-44.7358048778714,1.50000424468862,6.8326556215113));
#3359=CARTESIAN_POINT('Ctrl Pts',(-44.3330075021904,1.50000424468862,6.97604020093496));
#3360=CARTESIAN_POINT('Ctrl Pts',(-44.1303004124773,1.50000424468862,7.04504995476646));
#3361=CARTESIAN_POINT('Ctrl Pts',(-43.7219662840761,1.50000424468862,7.17808841752429));
#3362=CARTESIAN_POINT('Ctrl Pts',(-43.5170844940724,1.50000424468862,7.24186840105371));
#3363=CARTESIAN_POINT('Ctrl Pts',(-43.107010875435,1.50000424468862,7.36402161595204));
#3364=CARTESIAN_POINT('Ctrl Pts',(-42.9016041135959,1.50000424468862,7.42246492070205));
#3365=CARTESIAN_POINT('Ctrl Pts',(-42.2845508414699,1.50000424468862,7.59042137367504));
#3366=CARTESIAN_POINT('Ctrl Pts',(-41.8719366383669,1.50000424468862,7.69261310357766));
#3367=CARTESIAN_POINT('Ctrl Pts',(-41.0446440327223,1.50000424468862,7.88028330663815));
#3368=CARTESIAN_POINT('Ctrl Pts',(-40.6299533000686,1.50000424468862,7.96575790042277));
#3369=CARTESIAN_POINT('Ctrl Pts',(-39.3832305879684,1.50000424468862,8.20096473155133));
#3370=CARTESIAN_POINT('Ctrl Pts',(-38.5485529379463,1.50000424468862,8.32951876556412));
#3371=CARTESIAN_POINT('Ctrl Pts',(-37.2929149715664,1.50000424468862,8.49336037753108));
#3372=CARTESIAN_POINT('Ctrl Pts',(-36.8737616841785,1.50000424468862,8.54311292039738));
#3373=CARTESIAN_POINT('Ctrl Pts',(-36.0344921391938,1.50000424468862,8.63490959633655));
#3374=CARTESIAN_POINT('Ctrl Pts',(-35.6143772910846,1.50000424468862,8.67696500794892));
#3375=CARTESIAN_POINT('Ctrl Pts',(-34.7734157326484,1.50000424468862,8.75521742500524));
#3376=CARTESIAN_POINT('Ctrl Pts',(-34.3525922942412,1.50000424468862,8.79160070265665));
#3377=CARTESIAN_POINT('Ctrl Pts',(-33.510295192155,1.50000424468862,8.85916226730201));
#3378=CARTESIAN_POINT('Ctrl Pts',(-33.0888144051685,1.50000424468862,8.89028354208506));
#3379=CARTESIAN_POINT('Ctrl Pts',(-31.8233820850184,1.50000424468862,8.97572285277626));
#3380=CARTESIAN_POINT('Ctrl Pts',(-30.9784103501772,1.50000424468862,9.02207604912839));
#3381=CARTESIAN_POINT('Ctrl Pts',(-29.2859136426566,1.50000424468862,9.09353706128219));
#3382=CARTESIAN_POINT('Ctrl Pts',(-28.4380681793794,1.50000424468862,9.11864626001917));
#3383=CARTESIAN_POINT('Ctrl Pts',(-26.7408102190484,1.50000424468862,9.14751365292547));
#3384=CARTESIAN_POINT('Ctrl Pts',(-25.8926280014397,1.50000424468862,9.15126154992858));
#3385=CARTESIAN_POINT('Ctrl Pts',(-24.196466356748,1.50000424468862,9.13751512655564));
#3386=CARTESIAN_POINT('Ctrl Pts',(-23.3486016456246,1.50000424468862,9.12001922212186));
#3387=CARTESIAN_POINT('Ctrl Pts',(-21.6533026593848,1.50000424468862,9.06386983730065));
#3388=CARTESIAN_POINT('Ctrl Pts',(-20.8059333011263,1.50000424468862,9.02520867128565));
#3389=CARTESIAN_POINT('Ctrl Pts',(-19.5350064906316,1.50000424468862,8.95141355489978));
#3390=CARTESIAN_POINT('Ctrl Pts',(-19.1115305199824,1.50000424468862,8.92413823918045));
#3391=CARTESIAN_POINT('Ctrl Pts',(-18.2652153631114,1.50000424468862,8.8647255713046));
#3392=CARTESIAN_POINT('Ctrl Pts',(-17.8422984792913,1.50000424468862,8.83259214057113));
#3393=CARTESIAN_POINT('Ctrl Pts',(-16.5743006753995,1.50000424468862,8.72967574504789));
#3394=CARTESIAN_POINT('Ctrl Pts',(-15.72988800375,1.50000424468862,8.65238116375449));
#3395=CARTESIAN_POINT('Ctrl Pts',(-13.198843265656,1.50000424468862,8.40060735977158));
#3396=CARTESIAN_POINT('Ctrl Pts',(-11.5143241645176,1.50000424468862,8.20628809518815));
#3397=CARTESIAN_POINT('Ctrl Pts',(-8.1474934174154,1.50000424468862,7.79735066775273));
#3398=CARTESIAN_POINT('Ctrl Pts',(-6.46516732482365,1.50000424468862,7.58278618092267));
#3399=CARTESIAN_POINT('Ctrl Pts',(-3.94077394457453,1.50000424468862,7.26934320881284));
#3400=CARTESIAN_POINT('Ctrl Pts',(-3.09914796278127,1.50000424468862,7.16625406252897));
#3401=CARTESIAN_POINT('Ctrl Pts',(-1.41525996229401,1.50000424468862,6.96660071619449));
#3402=CARTESIAN_POINT('Ctrl Pts',(-0.572995336836428,1.50000424468862,6.87006947964638));
#3403=CARTESIAN_POINT('Ctrl Pts',(0.691132836996335,1.50000424468862,6.73276694004229));
#3404=CARTESIAN_POINT('Ctrl Pts',(1.11263597424435,1.50000424468862,6.6883027790284));
#3405=CARTESIAN_POINT('Ctrl Pts',(1.95592373084958,1.50000424468862,6.60226135719316));
#3406=CARTESIAN_POINT('Ctrl Pts',(2.37771906724245,1.50000424468862,6.56079404822635));
#3407=CARTESIAN_POINT('Ctrl Pts',(3.64350089097926,1.50000424468862,6.44045159867955));
#3408=CARTESIAN_POINT('Ctrl Pts',(4.48783416472058,1.50000424468862,6.3651333228694));
#3409=CARTESIAN_POINT('Ctrl Pts',(6.17690063171921,1.50000424468862,6.21859844147724));
#3410=CARTESIAN_POINT('Ctrl Pts',(7.02162882253013,1.50000424468862,6.14733057126028));
#3411=CARTESIAN_POINT('Ctrl Pts',(8.71087766779818,1.50000424468862,6.0026664064732));
#3412=CARTESIAN_POINT('Ctrl Pts',(9.55541256297313,1.50000424468862,5.92928624336249));
#3413=CARTESIAN_POINT('Ctrl Pts',(11.2436012924755,1.50000424468862,5.77400940558164));
#3414=CARTESIAN_POINT('Ctrl Pts',(12.0873886915773,1.50000424468862,5.69211951289022));
#3415=CARTESIAN_POINT('Ctrl Pts',(13.7727791084152,1.50000424468862,5.51285655268981));
#3416=CARTESIAN_POINT('Ctrl Pts',(14.6144462244022,1.50000424468862,5.41550723650472));
#3417=CARTESIAN_POINT('Ctrl Pts',(15.8745706893567,1.50000424468862,5.2518376377522));
#3418=CARTESIAN_POINT('Ctrl Pts',(16.2942164913156,1.50000424468862,5.194334903692));
#3419=CARTESIAN_POINT('Ctrl Pts',(17.1325605534117,1.50000424468862,5.07227422446284));
#3420=CARTESIAN_POINT('Ctrl Pts',(17.5512592043762,1.50000424468862,5.00771918949975));
#3421=CARTESIAN_POINT('Ctrl Pts',(18.1784675269534,1.50000424468862,4.9046347381739));
#3422=CARTESIAN_POINT('Ctrl Pts',(18.3873969138115,1.50000424468862,4.86923043909388));
#3423=CARTESIAN_POINT('Ctrl Pts',(18.7005631843819,1.50000424468862,4.81442776426905));
#3424=CARTESIAN_POINT('Ctrl Pts',(18.8049139660963,1.50000424468862,4.79587744987488));
#3425=CARTESIAN_POINT('Ctrl Pts',(19.0135364870674,1.50000424468862,4.75818828779729));
#3426=CARTESIAN_POINT('Ctrl Pts',(19.1178090657383,1.50000424468862,4.73905213336367));
#3427=CARTESIAN_POINT('Ctrl Pts',(19.3262686371032,1.50000424468862,4.70015679239322));
#3428=CARTESIAN_POINT('Ctrl Pts',(19.430418771527,1.50000424468862,4.68043767856379));
#3429=CARTESIAN_POINT('Ctrl Pts',(19.6384865349788,1.50000424468862,4.64020578699138));
#3430=CARTESIAN_POINT('Ctrl Pts',(19.7424000925144,1.50000424468862,4.61967928244251));
#3431=CARTESIAN_POINT('Ctrl Pts',(20.0536422980033,1.50000424468862,4.55639894428754));
#3432=CARTESIAN_POINT('Ctrl Pts',(20.2604666189451,1.50000424468862,4.5119242877194));
#3433=CARTESIAN_POINT('Ctrl Pts',(20.6720192733516,1.50000424468862,4.41582318750738));
#3434=CARTESIAN_POINT('Ctrl Pts',(20.876742698695,1.50000424468862,4.36417999658545));
#3435=CARTESIAN_POINT('Ctrl Pts',(21.2834003998586,1.50000424468862,4.25137663415474));
#3436=CARTESIAN_POINT('Ctrl Pts',(21.4853308265756,1.50000424468862,4.19020332993022));
#3437=CARTESIAN_POINT('Ctrl Pts',(21.8858633741466,1.50000424468862,4.05650003242997));
#3438=CARTESIAN_POINT('Ctrl Pts',(22.0844642714823,1.50000424468862,3.98396462045235));
#3439=CARTESIAN_POINT('Ctrl Pts',(22.4780037152932,1.50000424468862,3.82640225072584));
#3440=CARTESIAN_POINT('Ctrl Pts',(22.6729727572114,1.50000424468862,3.74136495201728));
#3441=CARTESIAN_POINT('Ctrl Pts',(22.9625022501059,1.50000424468862,3.60416799032947));
#3442=CARTESIAN_POINT('Ctrl Pts',(23.0582039529822,1.50000424468862,3.55698868386574));
#3443=CARTESIAN_POINT('Ctrl Pts',(23.2480654317315,1.50000424468862,3.45977570935616));
#3444=CARTESIAN_POINT('Ctrl Pts',(23.3422185562957,1.50000424468862,3.40974593973871));
#3445=CARTESIAN_POINT('Ctrl Pts',(23.48231624516,1.50000424468862,3.33262936836403));
#3446=CARTESIAN_POINT('Ctrl Pts',(23.5288269086232,1.50000424468862,3.30657870843009));
#3447=CARTESIAN_POINT('Ctrl Pts',(23.6214777127621,1.50000424468862,3.25379921372457));
#3448=CARTESIAN_POINT('Ctrl Pts',(23.6676163291091,1.50000424468862,3.22706758916978));
#3449=CARTESIAN_POINT('Ctrl Pts',(23.7365562716072,1.50000424468862,3.18647965905807));
#3450=CARTESIAN_POINT('Ctrl Pts',(23.7594884622631,1.50000424468862,3.17286287905752));
#3451=CARTESIAN_POINT('Ctrl Pts',(23.805268896492,1.50000424468862,3.14547566219199));
#3452=CARTESIAN_POINT('Ctrl Pts',(23.8281202947054,1.50000424468862,3.13171099952304));
#3453=CARTESIAN_POINT('Ctrl Pts',(23.8965947007905,1.50000424468862,3.09027096277851));
#3454=CARTESIAN_POINT('Ctrl Pts',(23.9421431991977,1.50000424468862,3.06245920626797));
#3455=CARTESIAN_POINT('Ctrl Pts',(24.0787585992021,1.50000424468862,2.97896881982385));
#3456=CARTESIAN_POINT('Ctrl Pts',(24.1697954746497,1.50000424468862,2.92323520931005));
#3457=CARTESIAN_POINT('Ctrl Pts',(24.3529430457551,1.50000424468862,2.81373335788034));
#3458=CARTESIAN_POINT('Ctrl Pts',(24.4450438892746,1.50000424468862,2.75993301037979));
#3459=CARTESIAN_POINT('Ctrl Pts',(24.7244481055146,1.50000424468862,2.60429339584203));
#3460=CARTESIAN_POINT('Ctrl Pts',(24.9149058159532,1.50000424468862,2.50796758924331));
#3461=CARTESIAN_POINT('Ctrl Pts',(25.1135772365769,1.50000424468862,2.4271963168569));
#3462=CARTESIAN_POINT('Ctrl Pts',(-54.4844548707889,-4.24468864876006E-6,
1.95915007643658));
#3463=CARTESIAN_POINT('Ctrl Pts',(-54.1631909828898,-4.24468864876006E-6,
2.24590494866024));
#3464=CARTESIAN_POINT('Ctrl Pts',(-53.8419270949909,-4.24468864876006E-6,
2.5326598208839));
#3465=CARTESIAN_POINT('Ctrl Pts',(-53.3600312631424,-4.24468864876006E-6,
2.96279212921941));
#3466=CARTESIAN_POINT('Ctrl Pts',(-53.199399319193,-4.24468864876006E-6,
3.10616956533124));
#3467=CARTESIAN_POINT('Ctrl Pts',(-52.878135431294,-4.24468864876006E-6,
3.39292443755491));
#3468=CARTESIAN_POINT('Ctrl Pts',(-52.7175034873445,-4.24468864876006E-6,
3.53630187366676));
#3469=CARTESIAN_POINT('Ctrl Pts',(-52.4765555714202,-4.24468864876006E-6,
3.75136802783449));
#3470=CARTESIAN_POINT('Ctrl Pts',(-52.3962395994455,-4.24468864876006E-6,
3.82305674589042));
#3471=CARTESIAN_POINT('Ctrl Pts',(-52.235607655496,-4.24468864876006E-6,
3.96643418200225));
#3472=CARTESIAN_POINT('Ctrl Pts',(-52.1552916835213,-4.24468864876006E-6,
4.03812290005816));
#3473=CARTESIAN_POINT('Ctrl Pts',(-51.9946597395718,-4.24468864876006E-6,
4.18150033616999));
#3474=CARTESIAN_POINT('Ctrl Pts',(-51.9144227402979,-4.24468864876006E-6,
4.25316422926206));
#3475=CARTESIAN_POINT('Ctrl Pts',(-51.8139290594534,-4.24468864876006E-6,
4.34280615803678));
#3476=CARTESIAN_POINT('Ctrl Pts',(-51.793869809635,-4.24468864876006E-6,
4.36072213130976));
#3477=CARTESIAN_POINT('Ctrl Pts',(-51.7637513201444,-4.24468864876006E-6,
4.38760540058075));
#3478=CARTESIAN_POINT('Ctrl Pts',(-51.7537118236476,-4.24468864876006E-6,
4.39656649033775));
#3479=CARTESIAN_POINT('Ctrl Pts',(-51.7336328306539,-4.24468864876006E-6,
4.41448866985173));
#3480=CARTESIAN_POINT('Ctrl Pts',(-51.723593334157,-4.24468864876006E-6,
4.42344975960873));
#3481=CARTESIAN_POINT('Ctrl Pts',(-51.7085340894118,-4.24468864876006E-6,
4.43689139424419));
#3482=CARTESIAN_POINT('Ctrl Pts',(-51.7035143411634,-4.24468864876006E-6,
4.44137193912269));
#3483=CARTESIAN_POINT('Ctrl Pts',(-51.6934748446665,-4.24468864876006E-6,
4.45033302887968));
#3484=CARTESIAN_POINT('Ctrl Pts',(-51.688438436341,-4.24468864876006E-6,
4.45482800098852));
#3485=CARTESIAN_POINT('Ctrl Pts',(-51.6784322599983,-4.24468864876006E-6,
4.46376023628484));
#3486=CARTESIAN_POINT('Ctrl Pts',(-51.6726924455922,-4.24468864919374E-6,
4.46888101943176));
#3487=CARTESIAN_POINT('Ctrl Pts',(-51.6618473995543,-4.24468864832638E-6,
4.47854149516085));
#3488=CARTESIAN_POINT('Ctrl Pts',(-51.6562970666484,-4.24468864876006E-6,
4.4834802833282));
#3489=CARTESIAN_POINT('Ctrl Pts',(-51.6399334159774,-4.24468864919374E-6,
4.49802163123191));
#3490=CARTESIAN_POINT('Ctrl Pts',(-51.6289156084215,-4.2446886500611E-6,
4.50778950698426));
#3491=CARTESIAN_POINT('Ctrl Pts',(-51.606953166536,-4.2446886500611E-6,
4.52721245996945));
#3492=CARTESIAN_POINT('Ctrl Pts',(-51.5959601033195,-4.24468864919374E-6,
4.53691088012528));
#3493=CARTESIAN_POINT('Ctrl Pts',(-51.5629454085781,-4.24468864615798E-6,
4.56596692908652));
#3494=CARTESIAN_POINT('Ctrl Pts',(-51.540888271787,-4.24468864832638E-6,
4.58528534624317));
#3495=CARTESIAN_POINT('Ctrl Pts',(-51.4966794380725,-4.24468864919374E-6,
4.62381739320071));
#3496=CARTESIAN_POINT('Ctrl Pts',(-51.4745277411724,-4.24468864876006E-6,
4.64303102300578));
#3497=CARTESIAN_POINT('Ctrl Pts',(-51.4079309999015,-4.24468864919374E-6,
4.70051440404672));
#3498=CARTESIAN_POINT('Ctrl Pts',(-51.3633443025652,-4.24468864832638E-6,
4.73862664451631));
#3499=CARTESIAN_POINT('Ctrl Pts',(-51.2290192229532,-4.2446886478927E-6,
4.85233079692795));
#3500=CARTESIAN_POINT('Ctrl Pts',(-51.1387054721567,-4.24468864919374E-6,
4.92729816849616));
#3501=CARTESIAN_POINT('Ctrl Pts',(-50.9566223990134,-4.24468864832638E-6,
5.07550122998796));
#3502=CARTESIAN_POINT('Ctrl Pts',(-50.8647517193264,-4.24468864919374E-6,
5.14881587934781));
#3503=CARTESIAN_POINT('Ctrl Pts',(-50.6798829713378,-4.24468864832638E-6,
5.29345560729514));
#3504=CARTESIAN_POINT('Ctrl Pts',(-50.5869592637586,-4.24468864876006E-6,
5.36472995902057));
#3505=CARTESIAN_POINT('Ctrl Pts',(-50.1197166576145,-4.24468864876006E-6,
5.71605669911536));
#3506=CARTESIAN_POINT('Ctrl Pts',(-49.7378925849801,-4.24468864876006E-6,
5.98082726797411));
#3507=CARTESIAN_POINT('Ctrl Pts',(-48.9598685421464,-4.24468864876006E-6,
6.47928168267429));
#3508=CARTESIAN_POINT('Ctrl Pts',(-48.563691410888,-4.24468864876006E-6,
6.71296978926406));
#3509=CARTESIAN_POINT('Ctrl Pts',(-47.7587612895418,-4.24468864876006E-6,
7.15109650890973));
#3510=CARTESIAN_POINT('Ctrl Pts',(-47.3500117097391,-4.24468864832638E-6,
7.35553976657944));
#3511=CARTESIAN_POINT('Ctrl Pts',(-46.5215827116132,-4.24468864919374E-6,
7.73727044476595));
#3512=CARTESIAN_POINT('Ctrl Pts',(-46.1019043152216,-4.24468864832638E-6,
7.91456257082263));
#3513=CARTESIAN_POINT('Ctrl Pts',(-45.4653047942148,-4.24468864876006E-6,
8.16183140099499));
#3514=CARTESIAN_POINT('Ctrl Pts',(-45.251923396063,-4.24468864876006E-6,
8.24114413294632));
#3515=CARTESIAN_POINT('Ctrl Pts',(-44.8229684642909,-4.24468864919374E-6,
8.39384005981013));
#3516=CARTESIAN_POINT('Ctrl Pts',(-44.6074708746446,-4.24468864876006E-6,
8.46719854180413));
#3517=CARTESIAN_POINT('Ctrl Pts',(-44.1741416095873,-4.24468864876006E-6,
8.60838058880916));
#3518=CARTESIAN_POINT('Ctrl Pts',(-43.9571016703052,-4.24468864876006E-6,
8.67594010437595));
#3519=CARTESIAN_POINT('Ctrl Pts',(-43.5234575547092,-4.24468864876006E-6,
8.80511452305223));
#3520=CARTESIAN_POINT('Ctrl Pts',(-43.3066250840536,-4.24468864876006E-6,
8.86680384442496));
#3521=CARTESIAN_POINT('Ctrl Pts',(-42.6563790465704,-4.24468864876006E-6,
9.04379513483447));
#3522=CARTESIAN_POINT('Ctrl Pts',(-42.2230742615554,-4.24468864876006E-6,
9.15107775210572));
#3523=CARTESIAN_POINT('Ctrl Pts',(-41.3571915732473,-4.24468864876006E-6,
9.34750214684944));
#3524=CARTESIAN_POINT('Ctrl Pts',(-40.9245979127559,-4.24468864876006E-6,
9.43663923062303));
#3525=CARTESIAN_POINT('Ctrl Pts',(-39.6281642620891,-4.24468864832638E-6,
9.68122664907806));
#3526=CARTESIAN_POINT('Ctrl Pts',(-38.7656559435773,-4.24468864876006E-6,
9.81391397360718));
#3527=CARTESIAN_POINT('Ctrl Pts',(-37.4754801380301,-4.24468864876006E-6,
9.98226303757803));
#3528=CARTESIAN_POINT('Ctrl Pts',(-37.0460149547959,-4.24468864832638E-6,
10.0332267077553));
#3529=CARTESIAN_POINT('Ctrl Pts',(-36.1884249609025,-4.24468864876006E-6,
10.1270272731659));
#3530=CARTESIAN_POINT('Ctrl Pts',(-35.760242601367,-4.24468864876006E-6,
10.1698805773202));
#3531=CARTESIAN_POINT('Ctrl Pts',(-34.9056087364515,-4.24468864876006E-6,
10.2494050421315));
#3532=CARTESIAN_POINT('Ctrl Pts',(-34.4788497239255,-4.24468864876006E-6,
10.2862989699105));
#3533=CARTESIAN_POINT('Ctrl Pts',(-33.6238680529587,-4.24468864876006E-6,
10.3548792395391));
#3534=CARTESIAN_POINT('Ctrl Pts',(-33.196172126081,-4.24468864876006E-6,
10.3864580004466));
#3535=CARTESIAN_POINT('Ctrl Pts',(-31.9117885142389,-4.24468864919374E-6,
10.4731786472994));
#3536=CARTESIAN_POINT('Ctrl Pts',(-31.0542760316985,-4.24468864876006E-6,
10.5202177700256));
#3537=CARTESIAN_POINT('Ctrl Pts',(-29.3366004343738,-4.24468864832638E-6,
10.5927418909748));
#3538=CARTESIAN_POINT('Ctrl Pts',(-28.4761609749882,-4.24468864876006E-6,
10.6182238039896));
#3539=CARTESIAN_POINT('Ctrl Pts',(-26.753736370895,-4.24468864876006E-6,
10.6475192366273));
#3540=CARTESIAN_POINT('Ctrl Pts',(-25.8929997337171,-4.24468864876006E-6,
10.6513223130449));
#3541=CARTESIAN_POINT('Ctrl Pts',(-24.1717819963686,-4.24468864876006E-6,
10.6373728238196));
#3542=CARTESIAN_POINT('Ctrl Pts',(-23.3114173125031,-4.24468864919374E-6,
10.6196186545521));
#3543=CARTESIAN_POINT('Ctrl Pts',(-21.5911789732551,-4.24468864832638E-6,
10.5626432619593));
#3544=CARTESIAN_POINT('Ctrl Pts',(-20.7314510230155,-4.24468864832638E-6,
10.5234188888955));
#3545=CARTESIAN_POINT('Ctrl Pts',(-19.441792216715,-4.24468864876006E-6,
10.448536103454));
#3546=CARTESIAN_POINT('Ctrl Pts',(-19.0122165523162,-4.24468864876006E-6,
10.4208665337269));
#3547=CARTESIAN_POINT('Ctrl Pts',(-18.1544471235408,-4.24468864876006E-6,
10.3606495016279));
#3548=CARTESIAN_POINT('Ctrl Pts',(-17.7260784044787,-4.24468864876006E-6,
10.3281004648967));
#3549=CARTESIAN_POINT('Ctrl Pts',(-16.4427004238879,-4.24468864919374E-6,
10.22393543127));
#3550=CARTESIAN_POINT('Ctrl Pts',(-15.5892290681904,-4.24468864876006E-6,
10.1458010040509));
#3551=CARTESIAN_POINT('Ctrl Pts',(-13.0347329463099,-4.24468864832638E-6,
9.89169386670957));
#3552=CARTESIAN_POINT('Ctrl Pts',(-11.3394541627929,-4.24468864876006E-6,
9.69608062098439));
#3553=CARTESIAN_POINT('Ctrl Pts',(-7.96064443919703,-4.24468864876006E-6,
9.28568863815111));
#3554=CARTESIAN_POINT('Ctrl Pts',(-6.27708160578794,-4.24468864876006E-6,
9.07095942198016));
#3555=CARTESIAN_POINT('Ctrl Pts',(-3.75757541004525,-4.24468864876006E-6,
8.75812347031837));
#3556=CARTESIAN_POINT('Ctrl Pts',(-2.91870084671988,-4.24468864876006E-6,
8.65537432408514));
#3557=CARTESIAN_POINT('Ctrl Pts',(-1.24247890505796,-4.24468864876006E-6,
8.45662995246558));
#3558=CARTESIAN_POINT('Ctrl Pts',(-0.405235409874857,-4.24468864919374E-6,
8.36067726430746));
#3559=CARTESIAN_POINT('Ctrl Pts',(0.850127280186599,-4.24468864876006E-6,
8.22432900839042));
#3560=CARTESIAN_POINT('Ctrl Pts',(1.26837633590489,-4.24468864876006E-6,
8.18020840080394));
#3561=CARTESIAN_POINT('Ctrl Pts',(2.10462599056565,-4.24468864876006E-6,
8.09488527340259));
#3562=CARTESIAN_POINT('Ctrl Pts',(2.5227769892274,-4.24468864876006E-6,
8.05377607757964));
#3563=CARTESIAN_POINT('Ctrl Pts',(3.77964826378803,-4.24468864832638E-6,
7.9342787051788));
#3564=CARTESIAN_POINT('Ctrl Pts',(4.61982975317104,-4.24468864876006E-6,
7.8593247970349));
#3565=CARTESIAN_POINT('Ctrl Pts',(6.30419371027295,-4.24468864876006E-6,
7.7131979034561));
#3566=CARTESIAN_POINT('Ctrl Pts',(7.14835481232514,-4.24468864876006E-6,
7.64197694110491));
#3567=CARTESIAN_POINT('Ctrl Pts',(8.84012652250938,-4.24468864919374E-6,
7.49709660838037));
#3568=CARTESIAN_POINT('Ctrl Pts',(9.68775000402986,-4.24468864876006E-6,
7.42345438745665));
#3569=CARTESIAN_POINT('Ctrl Pts',(11.3860364236348,-4.24468864876006E-6,
7.26724848287081));
#3570=CARTESIAN_POINT('Ctrl Pts',(12.2368321119163,-4.24468864876006E-6,
7.18469404650909));
#3571=CARTESIAN_POINT('Ctrl Pts',(13.9406290199073,-4.24468864876006E-6,
7.00347272943309));
#3572=CARTESIAN_POINT('Ctrl Pts',(14.7936906554792,-4.24468864876006E-6,
6.90483476041796));
#3573=CARTESIAN_POINT('Ctrl Pts',(16.0747472355423,-4.24468864876006E-6,
6.73844570620125));
#3574=CARTESIAN_POINT('Ctrl Pts',(16.5020121097752,-4.24468864876006E-6,
6.67990457867625));
#3575=CARTESIAN_POINT('Ctrl Pts',(17.3570012957737,-4.24468864876006E-6,
6.55542036632586));
#3576=CARTESIAN_POINT('Ctrl Pts',(17.7847256564825,-4.24468864832638E-6,
6.48948086722424));
#3577=CARTESIAN_POINT('Ctrl Pts',(18.4266373375988,-4.24468864876006E-6,
6.38397980612089));
#3578=CARTESIAN_POINT('Ctrl Pts',(18.6406621440251,-4.24468864919374E-6,
6.34771315743955));
#3579=CARTESIAN_POINT('Ctrl Pts',(18.961778659762,-4.24468864876006E-6,
6.29151922355206));
#3580=CARTESIAN_POINT('Ctrl Pts',(19.0688307191644,-4.24468864919374E-6,
6.27248885679318));
#3581=CARTESIAN_POINT('Ctrl Pts',(19.2829609602867,-4.24468864832638E-6,
6.23380468529344));
#3582=CARTESIAN_POINT('Ctrl Pts',(19.3900597260118,-4.24468864919374E-6,
6.21415013547148));
#3583=CARTESIAN_POINT('Ctrl Pts',(19.6042007391548,-4.24468864876006E-6,
6.17419439260278));
#3584=CARTESIAN_POINT('Ctrl Pts',(19.7112461085491,-4.24468864876006E-6,
6.15392907336129));
#3585=CARTESIAN_POINT('Ctrl Pts',(19.9272264302374,-4.24468864876006E-6,
6.11216767492095));
#3586=CARTESIAN_POINT('Ctrl Pts',(20.0357728617059,-4.24468864876006E-6,
6.09072923957392));
#3587=CARTESIAN_POINT('Ctrl Pts',(20.3635143902835,-4.24468864876006E-6,
6.02409562830664));
#3588=CARTESIAN_POINT('Ctrl Pts',(20.5844261589125,-4.24468864876006E-6,
5.97663687543248));
#3589=CARTESIAN_POINT('Ctrl Pts',(21.0302539801377,-4.24468864876006E-6,
5.87253369180135));
#3590=CARTESIAN_POINT('Ctrl Pts',(21.2551250275804,-4.24468864876006E-6,
5.8158678012648));
#3591=CARTESIAN_POINT('Ctrl Pts',(21.706930268158,-4.24468864876006E-6,
5.69054314971047));
#3592=CARTESIAN_POINT('Ctrl Pts',(21.9338439714855,-4.24468864876006E-6,
5.62185840913194));
#3593=CARTESIAN_POINT('Ctrl Pts',(22.3872744277703,-4.24468864876006E-6,
5.47049881303899));
#3594=CARTESIAN_POINT('Ctrl Pts',(22.6137579556259,-4.24468864876006E-6,
5.3878160953161));
#3595=CARTESIAN_POINT('Ctrl Pts',(23.0637791743541,-4.24468864876006E-6,
5.20764012428314));
#3596=CARTESIAN_POINT('Ctrl Pts',(23.2873232366555,-4.24468864919374E-6,
5.11014492079912));
#3597=CARTESIAN_POINT('Ctrl Pts',(23.6188171790401,-4.24468864876006E-6,
4.95306204865404));
#3598=CARTESIAN_POINT('Ctrl Pts',(23.7283127561718,-4.24468864876006E-6,
4.89908055545908));
#3599=CARTESIAN_POINT('Ctrl Pts',(23.9452217954513,-4.24468864876006E-6,
4.78801861755573));
#3600=CARTESIAN_POINT('Ctrl Pts',(24.052627331722,-4.24468864919374E-6,
4.73094334456363));
#3601=CARTESIAN_POINT('Ctrl Pts',(24.2121137015532,-4.24468864919374E-6,
4.64315427997084));
#3602=CARTESIAN_POINT('Ctrl Pts',(24.2650059892836,-4.24468864876006E-6,
4.6135287181131));
#3603=CARTESIAN_POINT('Ctrl Pts',(24.370247935397,-4.24468864876006E-6,
4.553576546795));
#3604=CARTESIAN_POINT('Ctrl Pts',(24.4225865320031,-4.24468864876006E-6,
4.52325171765904));
#3605=CARTESIAN_POINT('Ctrl Pts',(24.5007207602356,-4.24468864876006E-6,
4.47725157068682));
#3606=CARTESIAN_POINT('Ctrl Pts',(24.5268414243549,-4.24468864919374E-6,
4.46174045687451));
#3607=CARTESIAN_POINT('Ctrl Pts',(24.5779990494117,-4.24468864832638E-6,
4.43113607626247));
#3608=CARTESIAN_POINT('Ctrl Pts',(24.6030407728393,-4.24468864876006E-6,
4.41605091568199));
#3609=CARTESIAN_POINT('Ctrl Pts',(24.6765864688913,-4.24468864919374E-6,
4.37154031068307));
#3610=CARTESIAN_POINT('Ctrl Pts',(24.724019847109,-4.24468864876006E-6,
4.3425731441949));
#3611=CARTESIAN_POINT('Ctrl Pts',(24.8616938128042,-4.24468864876006E-6,
4.25843914221016));
#3612=CARTESIAN_POINT('Ctrl Pts',(24.9483601377191,-4.24468864876006E-6,
4.20540803699128));
#3613=CARTESIAN_POINT('Ctrl Pts',(25.1139167318624,-4.24468864876006E-6,
4.10642432159279));
#3614=CARTESIAN_POINT('Ctrl Pts',(25.1927679440333,-4.24468864876006E-6,
4.06045407352152));
#3615=CARTESIAN_POINT('Ctrl Pts',(25.4191698874029,-4.24468864876006E-6,
3.93433064558436));
#3616=CARTESIAN_POINT('Ctrl Pts',(25.5560295617271,-4.24468864876006E-6,
3.86643808531681));
#3617=CARTESIAN_POINT('Ctrl Pts',(25.6783212705344,-4.24468864876006E-6,
3.8168328320339));
#3618=CARTESIAN_POINT('',(0.,0.,0.));
#3619=CARTESIAN_POINT('Origin',(25.5182217655705,0.,-1.87222413531758));
#3620=CARTESIAN_POINT('',(25.5182217655705,0.,-3.87222413531759));
#3621=CARTESIAN_POINT('Origin',(25.5182217655705,0.,-1.87222413531758));
#3622=CARTESIAN_POINT('',(25.5182217655705,1.5,-3.87222413531759));
#3623=CARTESIAN_POINT('',(25.5182217655705,0.,-3.87222413531759));
#3624=CARTESIAN_POINT('Origin',(25.5182217655705,1.5,-1.87222413531758));
#3625=CARTESIAN_POINT('Ctrl Pts',(-31.0084166862739,0.499999999999999,2.67704093130204));
#3626=CARTESIAN_POINT('Ctrl Pts',(-31.0084166862739,-0.219999999999999,
2.67704093130204));
#3627=CARTESIAN_POINT('Ctrl Pts',(-28.2076463187592,0.499999999999999,5.17696258174617));
#3628=CARTESIAN_POINT('Ctrl Pts',(-28.2076463187592,-0.219999999999999,
5.17696258174617));
#3629=CARTESIAN_POINT('Ctrl Pts',(-21.482456130384,0.499999999999999,6.37819210999435));
#3630=CARTESIAN_POINT('Ctrl Pts',(-21.482456130384,-0.219999999999999,6.37819210999435));
#3631=CARTESIAN_POINT('Ctrl Pts',(-10.4420666215006,0.499999999999999,6.51321702489205));
#3632=CARTESIAN_POINT('Ctrl Pts',(-10.4420666215006,-0.219999999999999,
6.51321702489205));
#3633=CARTESIAN_POINT('Ctrl Pts',(0.282701922195941,0.499999999999999,4.72397216873886));
#3634=CARTESIAN_POINT('Ctrl Pts',(0.282701922195941,-0.219999999999999,
4.72397216873886));
#3635=CARTESIAN_POINT('Ctrl Pts',(8.69351499070982,0.499999999999999,4.31367676768492));
#3636=CARTESIAN_POINT('Ctrl Pts',(8.69351499070982,-0.219999999999999,4.31367676768492));
#3637=CARTESIAN_POINT('Ctrl Pts',(12.1517585870304,0.499999999999999,3.62923948763913));
#3638=CARTESIAN_POINT('Ctrl Pts',(12.1517585870304,-0.219999999999999,3.62923948763913));
#3639=CARTESIAN_POINT('Ctrl Pts',(12.3457959310433,0.499999999999999,3.58626341940775));
#3640=CARTESIAN_POINT('Ctrl Pts',(12.3457959310433,-0.219999999999999,3.58626341940775));
#3641=CARTESIAN_POINT('',(12.3457959311297,0.,3.58626341938894));
#3642=CARTESIAN_POINT('',(12.3457959979746,0.500000312196434,3.58626372434223));
#3643=CARTESIAN_POINT('',(12.3457959311296,1.5,3.58626341938861));
#3644=CARTESIAN_POINT('',(-31.0084166020303,0.499999717221561,2.67704086144519));
#3645=CARTESIAN_POINT('Ctrl Pts',(12.3457959311296,0.499999999999999,3.58626341938861));
#3646=CARTESIAN_POINT('Ctrl Pts',(12.1517585870946,0.499999999999999,3.62923948762642));
#3647=CARTESIAN_POINT('Ctrl Pts',(8.69351499074593,0.499999999999999,4.31367676768316));
#3648=CARTESIAN_POINT('Ctrl Pts',(0.282701922195941,0.499999999999999,4.72397216873886));
#3649=CARTESIAN_POINT('Ctrl Pts',(-10.4420666215006,0.499999999999999,6.51321702489205));
#3650=CARTESIAN_POINT('Ctrl Pts',(-21.4824561267119,0.499999999999999,6.37819211003926));
#3651=CARTESIAN_POINT('Ctrl Pts',(-28.2076463113667,0.499999999999999,5.1769625830666));
#3652=CARTESIAN_POINT('Ctrl Pts',(-31.008416677683,0.499999994355063,2.67704093897015));
#3653=CARTESIAN_POINT('',(-31.0084166862739,0.,2.67704093130204));
#3654=CARTESIAN_POINT('',(-31.0084166862739,1.5,2.67704093130204));
#3655=CARTESIAN_POINT('Ctrl Pts',(-31.0084166862739,0.,2.67704093130204));
#3656=CARTESIAN_POINT('Ctrl Pts',(-28.2076463187592,0.,5.17696258174617));
#3657=CARTESIAN_POINT('Ctrl Pts',(-21.482456130384,0.,6.37819210999435));
#3658=CARTESIAN_POINT('Ctrl Pts',(-10.4420666215006,0.,6.51321702489205));
#3659=CARTESIAN_POINT('Ctrl Pts',(0.282701922195941,0.,4.72397216873886));
#3660=CARTESIAN_POINT('Ctrl Pts',(8.69351499074223,0.,4.31367676768334));
#3661=CARTESIAN_POINT('Ctrl Pts',(12.151758587088,0.,3.62923948762772));
#3662=CARTESIAN_POINT('Ctrl Pts',(12.3457959311297,0.,3.58626341938894));
#3663=CARTESIAN_POINT('Ctrl Pts',(15.4777909450074,1.5,2.26366898793832));
#3664=CARTESIAN_POINT('Ctrl Pts',(15.4777909450074,-0.660000000000002,2.26366898793832));
#3665=CARTESIAN_POINT('Ctrl Pts',(15.604589304325,1.5,2.22082970559645));
#3666=CARTESIAN_POINT('Ctrl Pts',(15.604589304325,-0.660000000000002,2.22082970559645));
#3667=CARTESIAN_POINT('Ctrl Pts',(16.0321425201824,1.5,2.16989877476718));
#3668=CARTESIAN_POINT('Ctrl Pts',(16.0321425201824,-0.660000000000002,2.16989877476718));
#3669=CARTESIAN_POINT('Ctrl Pts',(16.380711317993,1.5,3.03159825743662));
#3670=CARTESIAN_POINT('Ctrl Pts',(16.380711317993,-0.660000000000002,3.03159825743662));
#3671=CARTESIAN_POINT('Ctrl Pts',(16.7818328065524,1.5,3.98512327200762));
#3672=CARTESIAN_POINT('Ctrl Pts',(16.7818328065524,-0.660000000000002,3.98512327200762));
#3673=CARTESIAN_POINT('Ctrl Pts',(18.0021442434375,1.5,3.42330192479396));
#3674=CARTESIAN_POINT('Ctrl Pts',(18.0021442434375,-0.660000000000002,3.42330192479396));
#3675=CARTESIAN_POINT('Ctrl Pts',(19.1270049692968,1.5,3.45147463333956));
#3676=CARTESIAN_POINT('Ctrl Pts',(19.1270049692968,-0.660000000000002,3.45147463333956));
#3677=CARTESIAN_POINT('Ctrl Pts',(21.1106762553254,1.5,2.59215126849901));
#3678=CARTESIAN_POINT('Ctrl Pts',(21.1106762553254,-0.660000000000002,2.59215126849901));
#3679=CARTESIAN_POINT('Ctrl Pts',(24.1154409179203,1.5,2.13122905062585));
#3680=CARTESIAN_POINT('Ctrl Pts',(24.1154409179203,-0.660000000000002,2.13122905062585));
#3681=CARTESIAN_POINT('Ctrl Pts',(28.7570716465227,1.5,2.48541219309353));
#3682=CARTESIAN_POINT('Ctrl Pts',(28.7570716465227,-0.660000000000002,2.48541219309353));
#3683=CARTESIAN_POINT('Ctrl Pts',(30.8610725977064,1.5,-4.32380575261494));
#3684=CARTESIAN_POINT('Ctrl Pts',(30.8610725977064,-0.660000000000002,-4.32380575261494));
#3685=CARTESIAN_POINT('Ctrl Pts',(29.2519383950227,1.5,-4.7724535583603));
#3686=CARTESIAN_POINT('Ctrl Pts',(29.2519383950227,-0.660000000000002,-4.7724535583603));
#3687=CARTESIAN_POINT('',(17.7057705722702,1.5,3.60431887284736));
#3688=CARTESIAN_POINT('',(29.2519383950227,1.5,-4.77245355836028));
#3689=CARTESIAN_POINT('Ctrl Pts',(17.7057705722702,1.5,3.60431887284736));
#3690=CARTESIAN_POINT('Ctrl Pts',(18.2596235045177,1.5,3.42974716334014));
#3691=CARTESIAN_POINT('Ctrl Pts',(19.1299826853614,1.5,3.45018469129812));
#3692=CARTESIAN_POINT('Ctrl Pts',(21.1106762553254,1.5,2.59215126849901));
#3693=CARTESIAN_POINT('Ctrl Pts',(24.1154409179203,1.5,2.13122905062585));
#3694=CARTESIAN_POINT('Ctrl Pts',(28.7570716465227,1.5,2.48541219309353));
#3695=CARTESIAN_POINT('Ctrl Pts',(30.8610725977064,1.5,-4.32380575261494));
#3696=CARTESIAN_POINT('Ctrl Pts',(29.2519383950227,1.5,-4.77245355836028));
#3697=CARTESIAN_POINT('',(15.5758189333363,0.50000155332938,2.23621039387092));
#3698=CARTESIAN_POINT('Ctrl Pts',(17.7057705722709,1.49999999999931,3.60431887284718));
#3699=CARTESIAN_POINT('Ctrl Pts',(17.7031110290994,1.49722275297065,3.6051571477229));
#3700=CARTESIAN_POINT('Ctrl Pts',(17.7004506633562,1.49444326036002,3.6059992825549));
#3701=CARTESIAN_POINT('Ctrl Pts',(17.6977896002535,1.491661645525,3.60684525708301));
#3702=CARTESIAN_POINT('Ctrl Pts',(17.6598094264402,1.45196089028633,3.61891947643783));
#3703=CARTESIAN_POINT('Ctrl Pts',(17.6216545449597,1.41182941608976,3.63178245853097));
#3704=CARTESIAN_POINT('Ctrl Pts',(17.5835382242194,1.37164748726708,3.64484827643156));
#3705=CARTESIAN_POINT('Ctrl Pts',(17.5391653937624,1.32486999456962,3.66005875087463));
#3706=CARTESIAN_POINT('Ctrl Pts',(17.4948445411659,1.27802412435748,3.67554478384865));
#3707=CARTESIAN_POINT('Ctrl Pts',(17.4508805310589,1.23170981145215,3.69044990780328));
#3708=CARTESIAN_POINT('Ctrl Pts',(17.390139775776,1.16772187360406,3.71104285381494));
#3709=CARTESIAN_POINT('Ctrl Pts',(17.3300783592064,1.10474858484553,3.73053128190524));
#3710=CARTESIAN_POINT('Ctrl Pts',(17.2714557074252,1.04437211368676,3.746748229346));
#3711=CARTESIAN_POINT('Ctrl Pts',(17.2288606109445,1.00050269570534,3.75853142952328));
#3712=CARTESIAN_POINT('Ctrl Pts',(17.1870235802448,0.958004253366488,3.76859067496704));
#3713=CARTESIAN_POINT('Ctrl Pts',(17.1462434201237,0.91748371187863,3.77607540849513));
#3714=CARTESIAN_POINT('Ctrl Pts',(17.1308987836395,0.902236763915967,3.77889174160487));
#3715=CARTESIAN_POINT('Ctrl Pts',(17.115703959382,0.8872698558268,3.78134315103857));
#3716=CARTESIAN_POINT('Ctrl Pts',(17.1006757019891,0.872615321519951,3.78338238638474));
#3717=CARTESIAN_POINT('Ctrl Pts',(17.0686358538502,0.841372241137127,3.7877299823237));
#3718=CARTESIAN_POINT('Ctrl Pts',(17.0368320316669,0.81103299831122,3.79027827290231));
#3719=CARTESIAN_POINT('Ctrl Pts',(17.0056623734324,0.782246495163689,3.79033388695513));
#3720=CARTESIAN_POINT('Ctrl Pts',(16.9771440878453,0.755908647259284,3.79038477033117));
#3721=CARTESIAN_POINT('Ctrl Pts',(16.9491574377736,0.730870613915962,3.78834731258798));
#3722=CARTESIAN_POINT('Ctrl Pts',(16.9220198105467,0.707629391615289,3.78366412357332));
#3723=CARTESIAN_POINT('Ctrl Pts',(16.8979570438198,0.687021543110594,3.77951156875136));
#3724=CARTESIAN_POINT('Ctrl Pts',(16.8773111036014,0.670182282643359,3.77375218638167));
#3725=CARTESIAN_POINT('Ctrl Pts',(16.8596132434589,0.656301257240817,3.7673887064672));
#3726=CARTESIAN_POINT('Ctrl Pts',(16.8517425657586,0.650128020690516,3.7645587089954));
#3727=CARTESIAN_POINT('Ctrl Pts',(16.8444549751791,0.644539864366037,3.76160908956875));
#3728=CARTESIAN_POINT('Ctrl Pts',(16.8377108992226,0.639465511443471,3.75862385138259));
#3729=CARTESIAN_POINT('Ctrl Pts',(16.8301153862163,0.633750523375398,3.75526172799965));
#3730=CARTESIAN_POINT('Ctrl Pts',(16.823208377781,0.628687637778199,3.75185624556522));
#3731=CARTESIAN_POINT('Ctrl Pts',(16.8169313605122,0.624174347799258,3.74853336303511));
#3732=CARTESIAN_POINT('Ctrl Pts',(16.7815195844566,0.598712634510066,3.72978733016992));
#3733=CARTESIAN_POINT('Ctrl Pts',(16.7484971453216,0.578077766495358,3.70423315774478));
#3734=CARTESIAN_POINT('Ctrl Pts',(16.7173105344503,0.561525876955449,3.67247601143094));
#3735=CARTESIAN_POINT('Ctrl Pts',(16.6960540920307,0.550244295625811,3.65083069848507));
#3736=CARTESIAN_POINT('Ctrl Pts',(16.6761897156968,0.541152670171255,3.62684519200596));
#3737=CARTESIAN_POINT('Ctrl Pts',(16.6575806498602,0.533786696249175,3.6013739187025));
#3738=CARTESIAN_POINT('Ctrl Pts',(16.6376871086567,0.525912292073837,3.57414451184149));
#3739=CARTESIAN_POINT('Ctrl Pts',(16.619225449201,0.520009984352785,3.54522278492793));
#3740=CARTESIAN_POINT('Ctrl Pts',(16.602024489444,0.515512535079858,3.51567962967423));
#3741=CARTESIAN_POINT('Ctrl Pts',(16.5814858836639,0.51014240812546,3.48040396902344));
#3742=CARTESIAN_POINT('Ctrl Pts',(16.5622765757694,0.506656585391937,3.44342095261399));
#3743=CARTESIAN_POINT('Ctrl Pts',(16.5443411772826,0.504350243957675,3.40642785852021));
#3744=CARTESIAN_POINT('Ctrl Pts',(16.5431424574651,0.50419609866866,3.40395540969025));
#3745=CARTESIAN_POINT('Ctrl Pts',(16.5419494305495,0.504047222090552,3.40148292861609));
#3746=CARTESIAN_POINT('Ctrl Pts',(16.5407620833152,0.503903403797068,3.39901092252946));
#3747=CARTESIAN_POINT('Ctrl Pts',(16.5264951398497,0.502175309939439,3.36930775730037));
#3748=CARTESIAN_POINT('Ctrl Pts',(16.5126214116979,0.501131296660439,3.33877520325719));
#3749=CARTESIAN_POINT('Ctrl Pts',(16.4992129271919,0.500508072838966,3.30825796373013));
#3750=CARTESIAN_POINT('Ctrl Pts',(16.4908673841387,0.500120173577757,3.28926380102513));
#3751=CARTESIAN_POINT('Ctrl Pts',(16.4827014884031,0.499895284473406,3.27027731286861));
#3752=CARTESIAN_POINT('Ctrl Pts',(16.4747329295069,0.499769922015154,3.25150626308357));
#3753=CARTESIAN_POINT('Ctrl Pts',(16.4679026502636,0.499662467128061,3.23541658948106));
#3754=CARTESIAN_POINT('Ctrl Pts',(16.4608038217544,0.499628622524833,3.21850215242504));
#3755=CARTESIAN_POINT('Ctrl Pts',(16.4538691941752,0.499633152943755,3.20186981087292));
#3756=CARTESIAN_POINT('Ctrl Pts',(16.4465521506316,0.499637933196501,3.18432026463122));
#3757=CARTESIAN_POINT('Ctrl Pts',(16.4394159727634,0.499685437619131,3.16708885086712));
#3758=CARTESIAN_POINT('Ctrl Pts',(16.4329679810904,0.499734274346846,3.1515094741843));
#3759=CARTESIAN_POINT('Ctrl Pts',(16.4326781541,0.499736469480235,3.15080920593255));
#3760=CARTESIAN_POINT('Ctrl Pts',(16.4323897151146,0.499738665310908,3.15011226221279));
#3761=CARTESIAN_POINT('Ctrl Pts',(16.4321027118697,0.499740859977208,3.14941876225688));
#3762=CARTESIAN_POINT('Ctrl Pts',(16.4189048123257,0.499841782130048,3.11752803309743));
#3763=CARTESIAN_POINT('Ctrl Pts',(16.4056285637068,0.499964068050572,3.08539406439388));
#3764=CARTESIAN_POINT('Ctrl Pts',(16.3923146363802,0.499993418608882,3.05341112999197));
#3765=CARTESIAN_POINT('Ctrl Pts',(16.3905041364871,0.499997409856647,3.04906191747964));
#3766=CARTESIAN_POINT('Ctrl Pts',(16.3885584669575,0.500000000000007,3.04439241037328));
#3767=CARTESIAN_POINT('Ctrl Pts',(16.386497303637,0.500000000000006,3.03945284932727));
#3768=CARTESIAN_POINT('Ctrl Pts',(16.3777142389215,0.500000000000002,3.01840430654475));
#3769=CARTESIAN_POINT('Ctrl Pts',(16.3668279599517,0.500013565738278,2.99243842907649));
#3770=CARTESIAN_POINT('Ctrl Pts',(16.355357683933,0.500028207045904,2.96547257823315));
#3771=CARTESIAN_POINT('Ctrl Pts',(16.3479004028895,0.500037725940273,2.94794100985699));
#3772=CARTESIAN_POINT('Ctrl Pts',(16.3401961527186,0.500047699457953,2.9299898633552));
#3773=CARTESIAN_POINT('Ctrl Pts',(16.3326784228899,0.500054695275253,2.91267644838095));
#3774=CARTESIAN_POINT('Ctrl Pts',(16.3286328985424,0.500058459942229,2.90335956104754));
#3775=CARTESIAN_POINT('Ctrl Pts',(16.3246417171666,0.500061362311546,2.89422674409416));
#3776=CARTESIAN_POINT('Ctrl Pts',(16.3207751647991,0.500062867507892,2.88543672368119));
#3777=CARTESIAN_POINT('Ctrl Pts',(16.2984479439476,0.500071559191861,2.83467917318227));
#3778=CARTESIAN_POINT('Ctrl Pts',(16.2750727227244,0.500028068253373,2.78349236485305));
#3779=CARTESIAN_POINT('Ctrl Pts',(16.2507208369999,0.500006270829282,2.73363070383891));
#3780=CARTESIAN_POINT('Ctrl Pts',(16.2465455961156,0.500002533562391,2.72508169667038));
#3781=CARTESIAN_POINT('Ctrl Pts',(16.2423066128638,0.500000000000009,2.71649975941386));
#3782=CARTESIAN_POINT('Ctrl Pts',(16.2380046463533,0.500000000000007,2.7078994039198));
#3783=CARTESIAN_POINT('Ctrl Pts',(16.2160115257873,0.499999999999997,2.66393145232615));
#3784=CARTESIAN_POINT('Ctrl Pts',(16.1923725125796,0.500031011240663,2.61947930368824));
#3785=CARTESIAN_POINT('Ctrl Pts',(16.1671669155192,0.500038395999784,2.57649896923451));
#3786=CARTESIAN_POINT('Ctrl Pts',(16.1537644249716,0.50004232267385,2.55364517510015));
#3787=CARTESIAN_POINT('Ctrl Pts',(16.1399190089963,0.500039569353616,2.53120874899483));
#3788=CARTESIAN_POINT('Ctrl Pts',(16.125647161097,0.500021921973862,2.50947625132159));
#3789=CARTESIAN_POINT('Ctrl Pts',(16.1171183833107,0.500011375996811,2.49648903027618));
#3790=CARTESIAN_POINT('Ctrl Pts',(16.108310702811,0.499999999999986,2.48355951018343));
#3791=CARTESIAN_POINT('Ctrl Pts',(16.0992240534471,0.49999999999999,2.47078446108149));
#3792=CARTESIAN_POINT('Ctrl Pts',(16.0798188371901,0.499999999999998,2.44350239256654));
#3793=CARTESIAN_POINT('Ctrl Pts',(16.0591401886511,0.500032153485344,2.41692570967048));
#3794=CARTESIAN_POINT('Ctrl Pts',(16.0371885635348,0.500034626496161,2.39199625974152));
#3795=CARTESIAN_POINT('Ctrl Pts',(16.0169673495177,0.500036904563537,2.36903195802482));
#3796=CARTESIAN_POINT('Ctrl Pts',(15.9952885015027,0.50000000000003,2.34703350101923));
#3797=CARTESIAN_POINT('Ctrl Pts',(15.9721147607565,0.500000000000017,2.32697564309227));
#3798=CARTESIAN_POINT('Ctrl Pts',(15.9690970350271,0.500000000000016,2.3243636731645));
#3799=CARTESIAN_POINT('Ctrl Pts',(15.9660539660289,0.499999447831871,2.32178460547913));
#3800=CARTESIAN_POINT('Ctrl Pts',(15.9629854828687,0.499998755868987,2.31924057762361));
#3801=CARTESIAN_POINT('Ctrl Pts',(15.9474963783552,0.49999526297531,2.30639882119796));
#3802=CARTESIAN_POINT('Ctrl Pts',(15.9312993972364,0.500000000000034,2.2943997687265));
#3803=CARTESIAN_POINT('Ctrl Pts',(15.9143698160608,0.500000000000026,2.28353887216815));
#3804=CARTESIAN_POINT('Ctrl Pts',(15.9079160821409,0.500000000000023,2.2793985844793));
#3805=CARTESIAN_POINT('Ctrl Pts',(15.9013558869196,0.500000796710013,2.27542369857025));
#3806=CARTESIAN_POINT('Ctrl Pts',(15.8946878996606,0.50000115650804,2.27163051661969));
#3807=CARTESIAN_POINT('Ctrl Pts',(15.8831363014348,0.500001779820908,2.26505922123644));
#3808=CARTESIAN_POINT('Ctrl Pts',(15.8713127070406,0.500000000000019,2.25906251116108));
#3809=CARTESIAN_POINT('Ctrl Pts',(15.8592065464433,0.500000000000015,2.25370333364518));
#3810=CARTESIAN_POINT('Ctrl Pts',(15.8484050624903,0.500000000000012,2.24892171279406));
#3811=CARTESIAN_POINT('Ctrl Pts',(15.8373786323162,0.499983033802094,2.24464763132202));
#3812=CARTESIAN_POINT('Ctrl Pts',(15.8261197469387,0.499988596289819,2.24092577040655));
#3813=CARTESIAN_POINT('Ctrl Pts',(15.8260310399079,0.499988640115806,2.24089644643532));
#3814=CARTESIAN_POINT('Ctrl Pts',(15.8259423255587,0.499988684421491,2.24086715909388));
#3815=CARTESIAN_POINT('Ctrl Pts',(15.8258536038921,0.499988729180149,2.24083790838682));
#3816=CARTESIAN_POINT('Ctrl Pts',(15.8191277861575,0.49999212224741,2.23862046892895));
#3817=CARTESIAN_POINT('Ctrl Pts',(15.8123599112164,0.499999999999994,2.23661356904048));
#3818=CARTESIAN_POINT('Ctrl Pts',(15.8055540048929,0.499999999999989,2.23480861085287));
#3819=CARTESIAN_POINT('Ctrl Pts',(15.7861201063075,0.499999999999977,2.22965465005735));
#3820=CARTESIAN_POINT('Ctrl Pts',(15.7663760877143,0.499999999999995,2.22614752151095));
#3821=CARTESIAN_POINT('Ctrl Pts',(15.7464171834751,0.499999999999999,2.22408394272492));
#3822=CARTESIAN_POINT('Ctrl Pts',(15.7330714101828,0.500000000000001,2.22270410471783));
#3823=CARTESIAN_POINT('Ctrl Pts',(15.7196296183475,0.499965185715635,2.22196957770925));
#3824=CARTESIAN_POINT('Ctrl Pts',(15.7061201902805,0.499946779332921,2.22181911498421));
#3825=CARTESIAN_POINT('Ctrl Pts',(15.6703952081703,0.499898104608135,2.22142122410876));
#3826=CARTESIAN_POINT('Ctrl Pts',(15.6345058507886,0.500000000000026,2.22511547817362));
#3827=CARTESIAN_POINT('Ctrl Pts',(15.5992847698687,0.500000000000013,2.23152789104314));
#3828=CARTESIAN_POINT('Ctrl Pts',(15.5914264811459,0.50000000000001,2.23295858511675));
#3829=CARTESIAN_POINT('Ctrl Pts',(15.5836014534938,0.500000633198017,2.23452449876141));
#3830=CARTESIAN_POINT('Ctrl Pts',(15.5758189333363,0.50000155333021,2.23621039387093));
#3831=CARTESIAN_POINT('',(15.5758189333363,0.,2.23621039387092));
#3832=CARTESIAN_POINT('',(15.5758189333363,0.,2.23621039387092));
#3833=CARTESIAN_POINT('',(29.2519383950227,0.,-4.77245355836028));
#3834=CARTESIAN_POINT('Ctrl Pts',(15.5758189333363,0.,2.23621039387092));
#3835=CARTESIAN_POINT('Ctrl Pts',(15.6655680769744,0.,2.21676717105701));
#3836=CARTESIAN_POINT('Ctrl Pts',(16.0491847574363,0.,2.21202901452892));
#3837=CARTESIAN_POINT('Ctrl Pts',(16.380711317993,0.,3.03159825743662));
#3838=CARTESIAN_POINT('Ctrl Pts',(16.7818328065524,0.,3.98512327200762));
#3839=CARTESIAN_POINT('Ctrl Pts',(18.0021442434375,0.,3.42330192479396));
#3840=CARTESIAN_POINT('Ctrl Pts',(19.1270049692968,0.,3.45147463333956));
#3841=CARTESIAN_POINT('Ctrl Pts',(21.1106762553254,0.,2.59215126849901));
#3842=CARTESIAN_POINT('Ctrl Pts',(24.1154409179203,0.,2.13122905062585));
#3843=CARTESIAN_POINT('Ctrl Pts',(28.7570716465227,0.,2.48541219309353));
#3844=CARTESIAN_POINT('Ctrl Pts',(30.8610725977064,0.,-4.32380575261494));
#3845=CARTESIAN_POINT('Ctrl Pts',(29.2519383950227,0.,-4.77245355836028));
#3846=CARTESIAN_POINT('',(29.2519383950227,1.5,-4.77245355836028));
#3847=CARTESIAN_POINT('Ctrl Pts',(29.2519383950227,1.5,-4.77245355836028));
#3848=CARTESIAN_POINT('Ctrl Pts',(29.2519383950227,-0.660000000000001,-4.77245355836028));
#3849=CARTESIAN_POINT('Ctrl Pts',(21.9641071366747,1.5,-6.80439688368832));
#3850=CARTESIAN_POINT('Ctrl Pts',(21.9641071366747,-0.660000000000001,-6.80439688368832));
#3851=CARTESIAN_POINT('Ctrl Pts',(23.672101274549,1.5,-2.84729812934541));
#3852=CARTESIAN_POINT('Ctrl Pts',(23.672101274549,-0.660000000000001,-2.84729812934541));
#3853=CARTESIAN_POINT('Ctrl Pts',(19.1613411950016,1.5,-3.33371436884934));
#3854=CARTESIAN_POINT('Ctrl Pts',(19.1613411950016,-0.660000000000001,-3.33371436884934));
#3855=CARTESIAN_POINT('Ctrl Pts',(17.2345397051744,1.5,-3.38352975816413));
#3856=CARTESIAN_POINT('Ctrl Pts',(17.2345397051744,-0.660000000000001,-3.38352975816413));
#3857=CARTESIAN_POINT('Ctrl Pts',(16.8377109321552,1.5,-5.12600200141825));
#3858=CARTESIAN_POINT('Ctrl Pts',(16.8377109321552,-0.660000000000001,-5.12600200141825));
#3859=CARTESIAN_POINT('',(16.8377109321552,0.,-5.12600200141825));
#3860=CARTESIAN_POINT('Ctrl Pts',(29.2519383950227,0.,-4.77245355836028));
#3861=CARTESIAN_POINT('Ctrl Pts',(21.9641071366747,0.,-6.80439688368832));
#3862=CARTESIAN_POINT('Ctrl Pts',(23.672101274549,0.,-2.84729812934541));
#3863=CARTESIAN_POINT('Ctrl Pts',(19.1613411950016,0.,-3.33371436884934));
#3864=CARTESIAN_POINT('Ctrl Pts',(17.2345397051744,0.,-3.38352975816413));
#3865=CARTESIAN_POINT('Ctrl Pts',(16.8377109321552,0.,-5.12600200141825));
#3866=CARTESIAN_POINT('',(16.8377109321552,1.5,-5.12600200141825));
#3867=CARTESIAN_POINT('',(16.8377109321552,1.5,-5.12600200141825));
#3868=CARTESIAN_POINT('Ctrl Pts',(29.2519383950227,1.5,-4.77245355836028));
#3869=CARTESIAN_POINT('Ctrl Pts',(21.9641071366747,1.5,-6.80439688368832));
#3870=CARTESIAN_POINT('Ctrl Pts',(23.672101274549,1.5,-2.84729812934541));
#3871=CARTESIAN_POINT('Ctrl Pts',(19.1613411950016,1.5,-3.33371436884934));
#3872=CARTESIAN_POINT('Ctrl Pts',(17.2345397051744,1.5,-3.38352975816413));
#3873=CARTESIAN_POINT('Ctrl Pts',(16.8377109321552,1.5,-5.12600200141825));
#3874=CARTESIAN_POINT('Ctrl Pts',(16.8377109321552,1.5,-5.12600200141825));
#3875=CARTESIAN_POINT('Ctrl Pts',(16.8377109321552,-0.660000000000001,-5.12600200141825));
#3876=CARTESIAN_POINT('Ctrl Pts',(15.1463411250383,1.5,-5.12119887067394));
#3877=CARTESIAN_POINT('Ctrl Pts',(15.1463411250383,-0.660000000000001,-5.12119887067394));
#3878=CARTESIAN_POINT('Ctrl Pts',(6.1690825674038,1.5,-5.20039638916375));
#3879=CARTESIAN_POINT('Ctrl Pts',(6.1690825674038,-0.660000000000001,-5.20039638916375));
#3880=CARTESIAN_POINT('Ctrl Pts',(-6.52362749092467,1.5,-5.5794658499804));
#3881=CARTESIAN_POINT('Ctrl Pts',(-6.52362749092467,-0.660000000000001,
-5.5794658499804));
#3882=CARTESIAN_POINT('Ctrl Pts',(-21.242818604027,1.5,-3.2191168533087));
#3883=CARTESIAN_POINT('Ctrl Pts',(-21.242818604027,-0.660000000000001,-3.2191168533087));
#3884=CARTESIAN_POINT('Ctrl Pts',(-28.1355316629927,1.5,0.120711630909182));
#3885=CARTESIAN_POINT('Ctrl Pts',(-28.1355316629927,-0.660000000000001,
0.120711630909182));
#3886=CARTESIAN_POINT('Ctrl Pts',(-31.0084166862739,1.5,2.67704093130204));
#3887=CARTESIAN_POINT('Ctrl Pts',(-31.0084166862739,-0.660000000000001,
2.67704093130204));
#3888=CARTESIAN_POINT('',(-30.2375369505402,1.5,2.02338898805065));
#3889=CARTESIAN_POINT('Ctrl Pts',(-31.0084164341763,0.49999948762028,2.67704070698238));
#3890=CARTESIAN_POINT('Ctrl Pts',(-30.8800361140849,0.670704692054994,2.5628062839063));
#3891=CARTESIAN_POINT('Ctrl Pts',(-30.7501472100187,0.84126783374662,2.45005907949001));
#3892=CARTESIAN_POINT('Ctrl Pts',(-30.6187111854204,1.01168753355088,2.33873890717364));
#3893=CARTESIAN_POINT('Ctrl Pts',(-30.4930248317139,1.1746522209994,2.23228843748564));
#3894=CARTESIAN_POINT('Ctrl Pts',(-30.365955714005,1.3374507451709,2.12717088547044));
#3895=CARTESIAN_POINT('Ctrl Pts',(-30.2375369505402,1.49999999999988,2.02338898805066));
#3896=CARTESIAN_POINT('Ctrl Pts',(16.8377109321552,1.5,-5.12600200141825));
#3897=CARTESIAN_POINT('Ctrl Pts',(15.1463411250383,1.5,-5.12119887067394));
#3898=CARTESIAN_POINT('Ctrl Pts',(6.1690825674038,1.5,-5.20039638916375));
#3899=CARTESIAN_POINT('Ctrl Pts',(-6.52362749092467,1.5,-5.5794658499804));
#3900=CARTESIAN_POINT('Ctrl Pts',(-20.9096607974693,1.5,-3.27254157538747));
#3901=CARTESIAN_POINT('Ctrl Pts',(-27.5202011308398,1.5,-0.172631746664609));
#3902=CARTESIAN_POINT('Ctrl Pts',(-30.2375369505402,1.5,2.02338898805065));
#3903=CARTESIAN_POINT('Ctrl Pts',(16.8377109321552,0.,-5.12600200141825));
#3904=CARTESIAN_POINT('Ctrl Pts',(15.1463411250383,0.,-5.12119887067394));
#3905=CARTESIAN_POINT('Ctrl Pts',(6.1690825674038,0.,-5.20039638916375));
#3906=CARTESIAN_POINT('Ctrl Pts',(-6.52362749092467,0.,-5.5794658499804));
#3907=CARTESIAN_POINT('Ctrl Pts',(-21.242818604027,0.,-3.2191168533087));
#3908=CARTESIAN_POINT('Ctrl Pts',(-28.1355316629927,0.,0.120711630909182));
#3909=CARTESIAN_POINT('Ctrl Pts',(-31.0084166862739,0.,2.67704093130204));
#3910=CARTESIAN_POINT('Origin',(1.14001967775083,1.5,4.86953436266123));
#3911=CARTESIAN_POINT('Ctrl Pts',(-30.2375369505396,1.49999999999999,2.02338898805013));
#3912=CARTESIAN_POINT('Ctrl Pts',(-30.2337952937897,1.5,2.02663560506344));
#3913=CARTESIAN_POINT('Ctrl Pts',(-30.2300593114649,1.49999999999999,2.02987242063508));
#3914=CARTESIAN_POINT('Ctrl Pts',(-30.2263138882049,1.49999999999999,2.03311253419974));
#3915=CARTESIAN_POINT('Ctrl Pts',(-30.041154668158,1.5,2.19329119995915));
#3916=CARTESIAN_POINT('Ctrl Pts',(-29.8513770723735,1.5,2.34550564113484));
#3917=CARTESIAN_POINT('Ctrl Pts',(-29.657068221066,1.5,2.49017675125092));
#3918=CARTESIAN_POINT('Ctrl Pts',(-29.4583612110577,1.49999999999999,2.63812247545394));
#3919=CARTESIAN_POINT('Ctrl Pts',(-29.2549154411805,1.49999999999999,2.77817943619801));
#3920=CARTESIAN_POINT('Ctrl Pts',(-29.0467943701774,1.49999999999999,2.91075212946208));
#3921=CARTESIAN_POINT('Ctrl Pts',(-28.985856418609,1.49999999999999,2.94956947901001));
#3922=CARTESIAN_POINT('Ctrl Pts',(-28.9245174562325,1.49999999999999,2.98774489874847));
#3923=CARTESIAN_POINT('Ctrl Pts',(-28.8627786201048,1.49999999999999,3.02528784234612));
#3924=CARTESIAN_POINT('Ctrl Pts',(-28.6690138779599,1.5,3.14311479280097));
#3925=CARTESIAN_POINT('Ctrl Pts',(-28.4710912906731,1.5,3.2548427970323));
#3926=CARTESIAN_POINT('Ctrl Pts',(-28.2693705204535,1.50000000000001,3.36065011064977));
#3927=CARTESIAN_POINT('Ctrl Pts',(-28.0602323419797,1.50000000000001,3.47034803027932));
#3928=CARTESIAN_POINT('Ctrl Pts',(-27.8470115970563,1.50000000000001,3.57368195430876));
#3929=CARTESIAN_POINT('Ctrl Pts',(-27.6301398763865,1.50000000000001,3.67089779862402));
#3930=CARTESIAN_POINT('Ctrl Pts',(-27.5380872989039,1.50000000000001,3.71216168039577));
#3931=CARTESIAN_POINT('Ctrl Pts',(-27.4453773123288,1.50000000000001,3.75232386587394));
#3932=CARTESIAN_POINT('Ctrl Pts',(-27.3520444442256,1.50000000000001,3.79140549983965));
#3933=CARTESIAN_POINT('Ctrl Pts',(-27.2326814421543,1.50000000000001,3.84138683279133));
#3934=CARTESIAN_POINT('Ctrl Pts',(-27.1125178794357,1.50000000000001,3.88949706274));
#3935=CARTESIAN_POINT('Ctrl Pts',(-26.9916583952716,1.5,3.93583843065075));
#3936=CARTESIAN_POINT('Ctrl Pts',(-26.8677028427576,1.5,3.98336692957956));
#3937=CARTESIAN_POINT('Ctrl Pts',(-26.7430131862653,1.5,4.0290352724924));
#3938=CARTESIAN_POINT('Ctrl Pts',(-26.6176845498461,1.5,4.07290501477839));
#3939=CARTESIAN_POINT('Ctrl Pts',(-26.5953628406859,1.49999999999999,4.08071845356));
#3940=CARTESIAN_POINT('Ctrl Pts',(-26.5730208653792,1.49999999999999,4.08847470468391));
#3941=CARTESIAN_POINT('Ctrl Pts',(-26.550659184495,1.49999999999999,4.09617393974249));
#3942=CARTESIAN_POINT('Ctrl Pts',(-26.3659847005078,1.49999999999999,4.15975825922633));
#3943=CARTESIAN_POINT('Ctrl Pts',(-26.179975006428,1.49999999999999,4.21950176210725));
#3944=CARTESIAN_POINT('Ctrl Pts',(-25.9929624158959,1.49999999999999,4.27567815256462));
#3945=CARTESIAN_POINT('Ctrl Pts',(-25.9080537125835,1.49999999999999,4.30118373193193));
#3946=CARTESIAN_POINT('Ctrl Pts',(-25.8229384188662,1.49999999999999,4.32595472533356));
#3947=CARTESIAN_POINT('Ctrl Pts',(-25.7376483120083,1.49999999999999,4.35002014717083));
#3948=CARTESIAN_POINT('Ctrl Pts',(-25.5174667344811,1.5,4.41214649147025));
#3949=CARTESIAN_POINT('Ctrl Pts',(-25.2956862586475,1.5,4.4697686002656));
#3950=CARTESIAN_POINT('Ctrl Pts',(-25.0726272188845,1.5,4.52327325815951));
#3951=CARTESIAN_POINT('Ctrl Pts',(-24.830594648481,1.5,4.58132905312924));
#3952=CARTESIAN_POINT('Ctrl Pts',(-24.587056772788,1.5,4.63453724241089));
#3953=CARTESIAN_POINT('Ctrl Pts',(-24.342435232932,1.5,4.68345442597066));
#3954=CARTESIAN_POINT('Ctrl Pts',(-24.0806904412321,1.5,4.73579576119788));
#3955=CARTESIAN_POINT('Ctrl Pts',(-23.8177051001542,1.5,4.78322501460086));
#3956=CARTESIAN_POINT('Ctrl Pts',(-23.554008139782,1.5,4.82648647475461));
#3957=CARTESIAN_POINT('Ctrl Pts',(-23.2405244203756,1.5,4.87791582538803));
#3958=CARTESIAN_POINT('Ctrl Pts',(-22.92603517214,1.5,4.9234558821029));
#3959=CARTESIAN_POINT('Ctrl Pts',(-22.6114439723032,1.5,4.96443227490802));
#3960=CARTESIAN_POINT('Ctrl Pts',(-22.5446347761331,1.5,4.97313436151018));
#3961=CARTESIAN_POINT('Ctrl Pts',(-22.4778210194986,1.5,4.9816308147111));
#3962=CARTESIAN_POINT('Ctrl Pts',(-22.4110114057897,1.5,4.98993457808753));
#3963=CARTESIAN_POINT('Ctrl Pts',(-22.1508063610361,1.50000000000001,5.02227544942385));
#3964=CARTESIAN_POINT('Ctrl Pts',(-21.8925698598374,1.5,5.05138331788897));
#3965=CARTESIAN_POINT('Ctrl Pts',(-21.6386197859862,1.5,5.07781979513669));
#3966=CARTESIAN_POINT('Ctrl Pts',(-21.3769007661508,1.5,5.10506502806082));
#3967=CARTESIAN_POINT('Ctrl Pts',(-21.1197360819527,1.5,5.12947999537432));
#3968=CARTESIAN_POINT('Ctrl Pts',(-20.8696606678661,1.5,5.15169330709646));
#3969=CARTESIAN_POINT('Ctrl Pts',(-20.8191072598628,1.5,5.15618378695709));
#3970=CARTESIAN_POINT('Ctrl Pts',(-20.7688435066458,1.5,5.16058413868542));
#3971=CARTESIAN_POINT('Ctrl Pts',(-20.7188902492778,1.5,5.16489923127004));
#3972=CARTESIAN_POINT('Ctrl Pts',(-20.5041147969358,1.5,5.18345209469855));
#3973=CARTESIAN_POINT('Ctrl Pts',(-20.2950635510776,1.5,5.20034230108586));
#3974=CARTESIAN_POINT('Ctrl Pts',(-20.0933847656336,1.5,5.21564597030981));
#3975=CARTESIAN_POINT('Ctrl Pts',(-19.8715555619165,1.5,5.23247868154627));
#3976=CARTESIAN_POINT('Ctrl Pts',(-19.6586456330018,1.5,5.24739212952468));
#3977=CARTESIAN_POINT('Ctrl Pts',(-19.4568491468652,1.5,5.26055530564244));
#3978=CARTESIAN_POINT('Ctrl Pts',(-19.3049736457191,1.5,5.2704621380548));
#3979=CARTESIAN_POINT('Ctrl Pts',(-19.1593931820414,1.5,5.27937921742333));
#3980=CARTESIAN_POINT('Ctrl Pts',(-19.0210433870338,1.5,5.28739765571153));
#3981=CARTESIAN_POINT('Ctrl Pts',(-18.9711489355537,1.5,5.29028942421827));
#3982=CARTESIAN_POINT('Ctrl Pts',(-18.9221953644963,1.5,5.29306443545563));
#3983=CARTESIAN_POINT('Ctrl Pts',(-18.8742268000768,1.5,5.29572728213782));
#3984=CARTESIAN_POINT('Ctrl Pts',(-18.864824040027,1.5,5.29624925123789));
#3985=CARTESIAN_POINT('Ctrl Pts',(-18.8554560953261,1.5,5.2967670756345));
#3986=CARTESIAN_POINT('Ctrl Pts',(-18.8461471198503,1.5,5.29727948613276));
#3987=CARTESIAN_POINT('Ctrl Pts',(-18.7334862426067,1.5,5.3034808792284));
#3988=CARTESIAN_POINT('Ctrl Pts',(-18.6287310561587,1.5,5.30893490230097));
#3989=CARTESIAN_POINT('Ctrl Pts',(-18.5299112214963,1.5,5.31385439992691));
#3990=CARTESIAN_POINT('Ctrl Pts',(-18.4256380647603,1.5,5.31904537751521));
#3991=CARTESIAN_POINT('Ctrl Pts',(-18.3279734082384,1.5,5.32364078378197));
#3992=CARTESIAN_POINT('Ctrl Pts',(-18.2346016229507,1.5,5.32783073841533));
#3993=CARTESIAN_POINT('Ctrl Pts',(-18.1369546918885,1.5,5.33221253544296));
#3994=CARTESIAN_POINT('Ctrl Pts',(-18.0440027361324,1.5,5.33615054430275));
#3995=CARTESIAN_POINT('Ctrl Pts',(-17.9530965415633,1.5,5.33980494028624));
#3996=CARTESIAN_POINT('Ctrl Pts',(-17.9025040122938,1.5,5.34183874157595));
#3997=CARTESIAN_POINT('Ctrl Pts',(-17.8525451081636,1.5,5.34378373847719));
#3998=CARTESIAN_POINT('Ctrl Pts',(-17.8027630804267,1.5,5.34566078906948));
#3999=CARTESIAN_POINT('Ctrl Pts',(-17.7855305147468,1.5,5.34631054961735));
#4000=CARTESIAN_POINT('Ctrl Pts',(-17.7683191431228,1.5,5.34695212794483));
#4001=CARTESIAN_POINT('Ctrl Pts',(-17.7511100182894,1.5,5.34758626185815));
#4002=CARTESIAN_POINT('Ctrl Pts',(-17.7336280300427,1.5,5.34823045043408));
#4003=CARTESIAN_POINT('Ctrl Pts',(-17.7161523646819,1.5,5.34886680123599));
#4004=CARTESIAN_POINT('Ctrl Pts',(-17.6986908876287,1.5,5.3494950560435));
#4005=CARTESIAN_POINT('Ctrl Pts',(-17.3035641688426,1.5,5.36371150863198));
#4006=CARTESIAN_POINT('Ctrl Pts',(-16.9144695187083,1.5,5.37383244203566));
#4007=CARTESIAN_POINT('Ctrl Pts',(-16.5308798263576,1.5,5.3802221035256));
#4008=CARTESIAN_POINT('Ctrl Pts',(-16.2250165106129,1.5,5.38531703461675));
#4009=CARTESIAN_POINT('Ctrl Pts',(-15.922653236192,1.5,5.38803851156023));
#4010=CARTESIAN_POINT('Ctrl Pts',(-15.6235224734428,1.5,5.38854751646289));
#4011=CARTESIAN_POINT('Ctrl Pts',(-15.2342893805637,1.5,5.38920984069437));
#4012=CARTESIAN_POINT('Ctrl Pts',(-14.8505224896553,1.5,5.38612774065209));
#4013=CARTESIAN_POINT('Ctrl Pts',(-14.4716416695502,1.5,5.37959707331161));
#4014=CARTESIAN_POINT('Ctrl Pts',(-14.0859965104277,1.5,5.37294981086904));
#4015=CARTESIAN_POINT('Ctrl Pts',(-13.7054134455504,1.5,5.36272969242992));
#4016=CARTESIAN_POINT('Ctrl Pts',(-13.3292800193233,1.5,5.34919404558174));
#4017=CARTESIAN_POINT('Ctrl Pts',(-12.9565439992755,1.5,5.33578065878022));
#4018=CARTESIAN_POINT('Ctrl Pts',(-12.5881775953025,1.5,5.31911110583216));
#4019=CARTESIAN_POINT('Ctrl Pts',(-12.2235841570957,1.5,5.29938532633141));
#4020=CARTESIAN_POINT('Ctrl Pts',(-11.9125827069805,1.5,5.28255906072566));
#4021=CARTESIAN_POINT('Ctrl Pts',(-11.6043350479086,1.5,5.26343720653592));
#4022=CARTESIAN_POINT('Ctrl Pts',(-11.2984729831696,1.5,5.2423417983655));
#4023=CARTESIAN_POINT('Ctrl Pts',(-11.0387538851364,1.5,5.22442888593114));
#4024=CARTESIAN_POINT('Ctrl Pts',(-10.7807545217096,1.5,5.20509175026844));
#4025=CARTESIAN_POINT('Ctrl Pts',(-10.5242437369439,1.5,5.18449881210053));
#4026=CARTESIAN_POINT('Ctrl Pts',(-10.1804515117854,1.5,5.15689883402645));
#4027=CARTESIAN_POINT('Ctrl Pts',(-9.83933390510173,1.5,5.12707624458748));
#4028=CARTESIAN_POINT('Ctrl Pts',(-9.50033155741444,1.5,5.0954487571781));
#4029=CARTESIAN_POINT('Ctrl Pts',(-9.27567015075047,1.5,5.07448879669666));
#4030=CARTESIAN_POINT('Ctrl Pts',(-9.05193787862125,1.5,5.05273488616363));
#4031=CARTESIAN_POINT('Ctrl Pts',(-8.82897326682209,1.5,5.03029627520487));
#4032=CARTESIAN_POINT('Ctrl Pts',(-8.44288843028761,1.5,4.99144164543124));
#4033=CARTESIAN_POINT('Ctrl Pts',(-8.05910111634218,1.5,4.95055906622723));
#4034=CARTESIAN_POINT('Ctrl Pts',(-7.67677701721786,1.5,4.90814164011349));
#4035=CARTESIAN_POINT('Ctrl Pts',(-7.4041297573418,1.5,4.87789244832203));
#4036=CARTESIAN_POINT('Ctrl Pts',(-7.13222678735648,1.5,4.84686119117315));
#4037=CARTESIAN_POINT('Ctrl Pts',(-6.86076721285879,1.5,4.81521112359619));
#4038=CARTESIAN_POINT('Ctrl Pts',(-6.8229722811227,1.5,4.8108045295546));
#4039=CARTESIAN_POINT('Ctrl Pts',(-6.78518594616242,1.5,4.80638592407432));
#4040=CARTESIAN_POINT('Ctrl Pts',(-6.7474073974805,1.5,4.80195573309565));
#4041=CARTESIAN_POINT('Ctrl Pts',(-6.73441476210259,1.5,4.80043212093879));
#4042=CARTESIAN_POINT('Ctrl Pts',(-6.72141925548236,1.5,4.79890669429121));
#4043=CARTESIAN_POINT('Ctrl Pts',(-6.70841347214424,1.5,4.79737859996483));
#4044=CARTESIAN_POINT('Ctrl Pts',(-6.48267459125147,1.5,4.770855760535));
#4045=CARTESIAN_POINT('Ctrl Pts',(-6.25456998290655,1.5,4.74361006590382));
#4046=CARTESIAN_POINT('Ctrl Pts',(-6.02781808108521,1.5,4.71618895197073));
#4047=CARTESIAN_POINT('Ctrl Pts',(-5.61980678153037,1.5,4.6668481339171));
#4048=CARTESIAN_POINT('Ctrl Pts',(-5.21617467425362,1.5,4.61694421711996));
#4049=CARTESIAN_POINT('Ctrl Pts',(-4.83856112378684,1.5,4.5698878566956));
#4050=CARTESIAN_POINT('Ctrl Pts',(-4.6969560423618,1.5,4.55224172153646));
#4051=CARTESIAN_POINT('Ctrl Pts',(-4.55900979339634,1.5,4.53499627493262));
#4052=CARTESIAN_POINT('Ctrl Pts',(-4.42586408354591,1.5,4.51832611180184));
#4053=CARTESIAN_POINT('Ctrl Pts',(-4.40427308746376,1.5,4.51562286715919));
#4054=CARTESIAN_POINT('Ctrl Pts',(-4.38280832834808,1.5,4.51293473531525));
#4055=CARTESIAN_POINT('Ctrl Pts',(-4.36147467664027,1.5,4.51026244236388));
#4056=CARTESIAN_POINT('Ctrl Pts',(-4.34931105189763,1.5,4.50873880407129));
#4057=CARTESIAN_POINT('Ctrl Pts',(-4.33719246839501,1.5,4.50722061789631));
#4058=CARTESIAN_POINT('Ctrl Pts',(-4.32511184432304,1.5,4.50570701714359));
#4059=CARTESIAN_POINT('Ctrl Pts',(-4.10118642391084,1.5,4.47765104231391));
#4060=CARTESIAN_POINT('Ctrl Pts',(-3.88867243419537,1.5,4.45097091827309));
#4061=CARTESIAN_POINT('Ctrl Pts',(-3.68522030236831,1.5,4.42546582810022));
#4062=CARTESIAN_POINT('Ctrl Pts',(-3.42827353994682,1.5,4.39325456402381));
#4063=CARTESIAN_POINT('Ctrl Pts',(-3.1857805977361,1.5,4.36291637676583));
#4064=CARTESIAN_POINT('Ctrl Pts',(-2.95301755734803,1.5,4.33396311712648));
#4065=CARTESIAN_POINT('Ctrl Pts',(-2.64467597250301,1.5,4.2956086861621));
#4066=CARTESIAN_POINT('Ctrl Pts',(-2.35340950786154,1.5,4.2596775987671));
#4067=CARTESIAN_POINT('Ctrl Pts',(-2.06824404682498,1.5,4.22496787940098));
#4068=CARTESIAN_POINT('Ctrl Pts',(-1.8533186349837,1.5,4.19880762597287));
#4069=CARTESIAN_POINT('Ctrl Pts',(-1.64186374211442,1.5,4.1733370064896));
#4070=CARTESIAN_POINT('Ctrl Pts',(-1.42916964311695,1.5,4.14805861485451));
#4071=CARTESIAN_POINT('Ctrl Pts',(-1.24078810701873,1.5,4.12566973679558));
#4072=CARTESIAN_POINT('Ctrl Pts',(-1.05143453978735,1.5,4.10343097364107));
#4073=CARTESIAN_POINT('Ctrl Pts',(-0.857832534542974,1.5,4.08103919940624));
#4074=CARTESIAN_POINT('Ctrl Pts',(-0.68880652471363,1.5,4.06148985513608));
#4075=CARTESIAN_POINT('Ctrl Pts',(-0.51654223225136,1.5,4.04182373011371));
#4076=CARTESIAN_POINT('Ctrl Pts',(-0.338855474791857,1.5,4.02187807261217));
#4077=CARTESIAN_POINT('Ctrl Pts',(-0.172282687709815,1.5,4.00317997823689));
#4078=CARTESIAN_POINT('Ctrl Pts',(-0.000944601626649944,1.5,3.98423570945314));
#4079=CARTESIAN_POINT('Ctrl Pts',(0.176962309038757,1.5,3.96495299846918));
#4080=CARTESIAN_POINT('Ctrl Pts',(0.351606668284712,1.5,3.94602390408086));
#4081=CARTESIAN_POINT('Ctrl Pts',(0.532581040071602,1.5,3.92676768274042));
#4082=CARTESIAN_POINT('Ctrl Pts',(0.72159670751355,1.5,3.90714994018427));
#4083=CARTESIAN_POINT('Ctrl Pts',(0.889047570336262,1.5,3.8897703866154));
#4084=CARTESIAN_POINT('Ctrl Pts',(1.06280953667672,1.5,3.87210711157171));
#4085=CARTESIAN_POINT('Ctrl Pts',(1.24407702413679,1.5,3.8541829909191));
#4086=CARTESIAN_POINT('Ctrl Pts',(1.26742117348904,1.5,3.85187467101361));
#4087=CARTESIAN_POINT('Ctrl Pts',(1.29088980907388,1.5,3.84956209597365));
#4088=CARTESIAN_POINT('Ctrl Pts',(1.31448548841964,1.5,3.8472453802817));
#4089=CARTESIAN_POINT('Ctrl Pts',(1.42899700200292,1.5,3.83600219391104));
#4090=CARTESIAN_POINT('Ctrl Pts',(1.54649813261794,1.5,3.82464411253794));
#4091=CARTESIAN_POINT('Ctrl Pts',(1.6672770820639,1.5,3.81314819462295));
#4092=CARTESIAN_POINT('Ctrl Pts',(1.68548104283269,1.5,3.81141551488294));
#4093=CARTESIAN_POINT('Ctrl Pts',(1.70375400162177,1.5,3.80968021475685));
#4094=CARTESIAN_POINT('Ctrl Pts',(1.72212820038232,1.5,3.80793925503593));
#4095=CARTESIAN_POINT('Ctrl Pts',(1.8950448493804,1.5,3.79155536124524));
#4096=CARTESIAN_POINT('Ctrl Pts',(2.07645857851809,1.5,3.77471937250263));
#4097=CARTESIAN_POINT('Ctrl Pts',(2.26533613202404,1.5,3.75753239704228));
#4098=CARTESIAN_POINT('Ctrl Pts',(2.45451985028614,1.5,3.74031756201867));
#4099=CARTESIAN_POINT('Ctrl Pts',(2.65119161904104,1.5,3.7227506958672));
#4100=CARTESIAN_POINT('Ctrl Pts',(2.85430796830265,1.5,3.7048805235274));
#4101=CARTESIAN_POINT('Ctrl Pts',(3.06086450365666,1.5,3.68670768368409));
#4102=CARTESIAN_POINT('Ctrl Pts',(3.27408576401215,1.5,3.66822109255634));
#4103=CARTESIAN_POINT('Ctrl Pts',(3.49286897045564,1.5,3.6494170293364));
#4104=CARTESIAN_POINT('Ctrl Pts',(3.72558179917576,1.5,3.62941573758061));
#4105=CARTESIAN_POINT('Ctrl Pts',(3.96458735551702,1.5,3.60905518307288));
#4106=CARTESIAN_POINT('Ctrl Pts',(4.20855252728194,1.5,3.58826965400713));
#4107=CARTESIAN_POINT('Ctrl Pts',(4.37184747684828,1.5,3.57435712749383));
#4108=CARTESIAN_POINT('Ctrl Pts',(4.53736426395281,1.5,3.56025287349266));
#4109=CARTESIAN_POINT('Ctrl Pts',(4.70470187755637,1.5,3.54592444027639));
#4110=CARTESIAN_POINT('Ctrl Pts',(4.98380030472694,1.5,3.52202638718263));
#4111=CARTESIAN_POINT('Ctrl Pts',(5.26774502017556,1.5,3.49754691833425));
#4112=CARTESIAN_POINT('Ctrl Pts',(5.55524949715075,1.5,3.47220567087764));
#4113=CARTESIAN_POINT('Ctrl Pts',(5.93341654493371,1.5,3.43887323432351));
#4114=CARTESIAN_POINT('Ctrl Pts',(6.31774234964862,1.5,3.40404822381377));
#4115=CARTESIAN_POINT('Ctrl Pts',(6.70527769826349,1.5,3.36700056442672));
#4116=CARTESIAN_POINT('Ctrl Pts',(7.04422598225608,1.5,3.33459773815535));
#4117=CARTESIAN_POINT('Ctrl Pts',(7.38562841725574,1.5,3.30048928723064));
#4118=CARTESIAN_POINT('Ctrl Pts',(7.72750891122856,1.5,3.26419008408891));
#4119=CARTESIAN_POINT('Ctrl Pts',(7.84926141411927,1.5,3.25126299724611));
#4120=CARTESIAN_POINT('Ctrl Pts',(7.97107458551754,1.5,3.23805844494137));
#4121=CARTESIAN_POINT('Ctrl Pts',(8.09285941000345,1.5,3.22455637168536));
#4122=CARTESIAN_POINT('Ctrl Pts',(8.37921768375685,1.5,3.19280832420898));
#4123=CARTESIAN_POINT('Ctrl Pts',(8.66543795848237,1.5,3.15943873922727));
#4124=CARTESIAN_POINT('Ctrl Pts',(8.95033395522809,1.5,3.12409127077656));
#4125=CARTESIAN_POINT('Ctrl Pts',(9.18845852070908,1.5,3.09454680310476));
#4126=CARTESIAN_POINT('Ctrl Pts',(9.42565794543148,1.5,3.06362062240277));
#4127=CARTESIAN_POINT('Ctrl Pts',(9.66124991551543,1.5,3.03114544574892));
#4128=CARTESIAN_POINT('Ctrl Pts',(9.886670020665,1.5,3.00007240988334));
#4129=CARTESIAN_POINT('Ctrl Pts',(10.1106183714759,1.5,2.96758081885689));
#4130=CARTESIAN_POINT('Ctrl Pts',(10.3325085538622,1.5,2.93356848320867));
#4131=CARTESIAN_POINT('Ctrl Pts',(10.5440562437169,1.5,2.90114149182236));
#4132=CARTESIAN_POINT('Ctrl Pts',(10.753733117056,1.5,2.86733205096079));
#4133=CARTESIAN_POINT('Ctrl Pts',(10.9610425166206,1.5,2.83209688558433));
#4134=CARTESIAN_POINT('Ctrl Pts',(11.1247121753544,1.5,2.80427891155754));
#4135=CARTESIAN_POINT('Ctrl Pts',(11.2869063881666,1.5,2.77557308549288));
#4136=CARTESIAN_POINT('Ctrl Pts',(11.4473864461662,1.5,2.74598048905742));
#4137=CARTESIAN_POINT('Ctrl Pts',(11.553597493978,1.5,2.72639512303711));
#4138=CARTESIAN_POINT('Ctrl Pts',(11.6591804005066,1.5,2.70647589362988));
#4139=CARTESIAN_POINT('Ctrl Pts',(11.76367159676,1.5,2.68594799574105));
#4140=CARTESIAN_POINT('Ctrl Pts',(11.7964550844154,1.5,2.67950749059649));
#4141=CARTESIAN_POINT('Ctrl Pts',(11.829131199191,1.5,2.67300742457918));
#4142=CARTESIAN_POINT('Ctrl Pts',(11.8616859025202,1.5,2.6664404037272));
#4143=CARTESIAN_POINT('Ctrl Pts',(12.0008154873567,1.5,2.63837481592222));
#4144=CARTESIAN_POINT('Ctrl Pts',(12.1378233663548,1.49999999999999,2.6089918119749));
#4145=CARTESIAN_POINT('Ctrl Pts',(12.2734880318177,1.5,2.57708405230406));
#4146=CARTESIAN_POINT('Ctrl Pts',(12.3720491713233,1.5,2.55390288614339));
#4147=CARTESIAN_POINT('Ctrl Pts',(12.4698925440469,1.5,2.52935494370487));
#4148=CARTESIAN_POINT('Ctrl Pts',(12.5673303176919,1.5,2.503028111913));
#4149=CARTESIAN_POINT('Ctrl Pts',(12.6536663943788,1.5,2.47970086126389));
#4150=CARTESIAN_POINT('Ctrl Pts',(12.7396841195956,1.5,2.45497733455598));
#4151=CARTESIAN_POINT('Ctrl Pts',(12.8255910274147,1.5,2.42853300000139));
#4152=CARTESIAN_POINT('Ctrl Pts',(12.9114979352338,1.5,2.40208866544679));
#4153=CARTESIAN_POINT('Ctrl Pts',(12.9972942860165,1.5,2.37392454644978));
#4154=CARTESIAN_POINT('Ctrl Pts',(13.0831746516526,1.5,2.34366516065363));
#4155=CARTESIAN_POINT('Ctrl Pts',(13.1659810649101,1.5,2.31448886189672));
#4156=CARTESIAN_POINT('Ctrl Pts',(13.248863365756,1.5,2.28335555594758));
#4157=CARTESIAN_POINT('Ctrl Pts',(13.3320214711795,1.5,2.25002943668965));
#4158=CARTESIAN_POINT('Ctrl Pts',(13.4134355307938,1.5,2.2174022544546));
#4159=CARTESIAN_POINT('Ctrl Pts',(13.4951139958824,1.50000000000001,2.18267346241825));
#4160=CARTESIAN_POINT('Ctrl Pts',(13.5772322422152,1.50000000000001,2.14557372974471));
#4161=CARTESIAN_POINT('Ctrl Pts',(13.6568886107536,1.50000000000001,2.10958623475434));
#4162=CARTESIAN_POINT('Ctrl Pts',(13.7369588186311,1.50000000000001,2.07136795327505));
#4163=CARTESIAN_POINT('Ctrl Pts',(13.8175907589904,1.50000000000001,2.03062519205916));
#4164=CARTESIAN_POINT('Ctrl Pts',(13.8337964027114,1.50000000000001,2.02243659248517));
#4165=CARTESIAN_POINT('Ctrl Pts',(13.8500246957313,1.50000000000001,2.014145855992));
#4166=CARTESIAN_POINT('Ctrl Pts',(13.8662767749019,1.50000000000001,2.00575034734995));
#4167=CARTESIAN_POINT('Ctrl Pts',(13.9081642812626,1.50000000000001,1.98411207461237));
#4168=CARTESIAN_POINT('Ctrl Pts',(13.950461030891,1.50000000000001,1.96165528000694));
#4169=CARTESIAN_POINT('Ctrl Pts',(13.9926697842201,1.5,1.93862227096309));
#4170=CARTESIAN_POINT('Ctrl Pts',(14.0142784190252,1.5,1.92683059644927));
#4171=CARTESIAN_POINT('Ctrl Pts',(14.0358641984505,1.5,1.91488871790894));
#4172=CARTESIAN_POINT('Ctrl Pts',(14.0573617100153,1.49999999999999,1.90283427700156));
#4173=CARTESIAN_POINT('Ctrl Pts',(14.0897595100142,1.49999999999999,1.88466764574106));
#4174=CARTESIAN_POINT('Ctrl Pts',(14.1213372809979,1.49999999999999,1.86659470623033));
#4175=CARTESIAN_POINT('Ctrl Pts',(14.1521991517948,1.5,1.84860499061564));
#4176=CARTESIAN_POINT('Ctrl Pts',(14.184396915122,1.5,1.82983656891176));
#4177=CARTESIAN_POINT('Ctrl Pts',(14.2158029519234,1.50000000000002,1.81113812163914));
#4178=CARTESIAN_POINT('Ctrl Pts',(14.2465771364748,1.50000000000001,1.79256971204494));
#4179=CARTESIAN_POINT('Ctrl Pts',(14.2814551303541,1.49999999999999,1.77152516169812));
#4180=CARTESIAN_POINT('Ctrl Pts',(14.3155518423707,1.49999999999999,1.75069273316637));
#4181=CARTESIAN_POINT('Ctrl Pts',(14.3491101294543,1.49999999999998,1.73017817585942));
#4182=CARTESIAN_POINT('Ctrl Pts',(14.3779858740141,1.49999999999998,1.71252610931982));
#4183=CARTESIAN_POINT('Ctrl Pts',(14.4064625536128,1.49999999999998,1.69510776450755));
#4184=CARTESIAN_POINT('Ctrl Pts',(14.4346889400213,1.49999999999999,1.67796712650023));
#4185=CARTESIAN_POINT('Ctrl Pts',(14.4984589258247,1.5,1.63924243016231));
#4186=CARTESIAN_POINT('Ctrl Pts',(14.5609266774462,1.49999999999999,1.60191409094533));
#4187=CARTESIAN_POINT('Ctrl Pts',(14.6235034279238,1.49999999999999,1.56612658872582));
#4188=CARTESIAN_POINT('Ctrl Pts',(14.6623030990163,1.49999999999999,1.54393714448749));
#4189=CARTESIAN_POINT('Ctrl Pts',(14.7010798634147,1.49999999999999,1.52237211616235));
#4190=CARTESIAN_POINT('Ctrl Pts',(14.7402377283426,1.49999999999999,1.50142071435942));
#4191=CARTESIAN_POINT('Ctrl Pts',(14.7758873808755,1.49999999999999,1.48234638035967));
#4192=CARTESIAN_POINT('Ctrl Pts',(14.8118524075414,1.49999999999999,1.46377995768135));
#4193=CARTESIAN_POINT('Ctrl Pts',(14.8484505281561,1.49999999999999,1.44575260484134));
#4194=CARTESIAN_POINT('Ctrl Pts',(14.8815568628569,1.49999999999999,1.42944522165149));
#4195=CARTESIAN_POINT('Ctrl Pts',(14.9151810332879,1.49999999999999,1.41357870584738));
#4196=CARTESIAN_POINT('Ctrl Pts',(14.9495737189396,1.5,1.39821557530277));
#4197=CARTESIAN_POINT('Ctrl Pts',(14.9693267160288,1.5,1.38939195867676));
#4198=CARTESIAN_POINT('Ctrl Pts',(14.9893335232394,1.5,1.38073514573342));
#4199=CARTESIAN_POINT('Ctrl Pts',(15.0096447310109,1.5,1.37226431791822));
#4200=CARTESIAN_POINT('Ctrl Pts',(15.0722269561691,1.5,1.34616428193956));
#4201=CARTESIAN_POINT('Ctrl Pts',(15.1378964880444,1.5,1.32173616111247));
#4202=CARTESIAN_POINT('Ctrl Pts',(15.206402740382,1.5,1.30048138533187));
#4203=CARTESIAN_POINT('Ctrl Pts',(15.2573606011224,1.5,1.28467118017042));
#4204=CARTESIAN_POINT('Ctrl Pts',(15.3098890700018,1.5,1.2706197125179));
#4205=CARTESIAN_POINT('Ctrl Pts',(15.3638774142426,1.5,1.2589237086481));
#4206=CARTESIAN_POINT('Ctrl Pts',(15.3824694154108,1.5,1.25489594819965));
#4207=CARTESIAN_POINT('Ctrl Pts',(15.4012344108101,1.5,1.25114715061918));
#4208=CARTESIAN_POINT('Ctrl Pts',(15.4201673421117,1.5,1.24770018911881));
#4209=CARTESIAN_POINT('Ctrl Pts',(15.4480170350895,1.5,1.24262982690376));
#4210=CARTESIAN_POINT('Ctrl Pts',(15.4761145444581,1.5,1.23824102619373));
#4211=CARTESIAN_POINT('Ctrl Pts',(15.5042043297991,1.5,1.23461144646394));
#4212=CARTESIAN_POINT('Ctrl Pts',(15.5318620946041,1.5,1.23103768962352));
#4213=CARTESIAN_POINT('Ctrl Pts',(15.5595122873754,1.5,1.2282001066137));
#4214=CARTESIAN_POINT('Ctrl Pts',(15.5869091734653,1.5,1.2261221612424));
#4215=CARTESIAN_POINT('Ctrl Pts',(15.6142008008716,1.5,1.22405219932561));
#4216=CARTESIAN_POINT('Ctrl Pts',(15.6412409879309,1.5,1.22273610252946));
#4217=CARTESIAN_POINT('Ctrl Pts',(15.6677862089015,1.5,1.22214489863002));
#4218=CARTESIAN_POINT('Ctrl Pts',(15.6945406231681,1.5,1.22154903566623));
#4219=CARTESIAN_POINT('Ctrl Pts',(15.7207921702355,1.5,1.2216894969672));
#4220=CARTESIAN_POINT('Ctrl Pts',(15.7462920004296,1.5,1.22248322281614));
#4221=CARTESIAN_POINT('Ctrl Pts',(15.7726196829026,1.5,1.22330271698386));
#4222=CARTESIAN_POINT('Ctrl Pts',(15.7981459809862,1.5,1.22481849422764));
#4223=CARTESIAN_POINT('Ctrl Pts',(15.8225985815198,1.5,1.22688296680944));
#4224=CARTESIAN_POINT('Ctrl Pts',(15.8316370729344,1.5,1.2276460642837));
#4225=CARTESIAN_POINT('Ctrl Pts',(15.84052888648,1.5,1.22848360035794));
#4226=CARTESIAN_POINT('Ctrl Pts',(15.8492603460339,1.5,1.22938635857439));
#4227=CARTESIAN_POINT('Ctrl Pts',(15.8752106760547,1.5,1.23206940068224));
#4228=CARTESIAN_POINT('Ctrl Pts',(15.9002189981378,1.5,1.23539390779828));
#4229=CARTESIAN_POINT('Ctrl Pts',(15.9242319250192,1.5,1.23919918936648));
#4230=CARTESIAN_POINT('Ctrl Pts',(15.9501886120697,1.5,1.24331249480788));
#4231=CARTESIAN_POINT('Ctrl Pts',(15.974982600101,1.5,1.24798743511524));
#4232=CARTESIAN_POINT('Ctrl Pts',(15.9986007079772,1.5,1.25305595421041));
#4233=CARTESIAN_POINT('Ctrl Pts',(16.0207226927192,1.5,1.25780340064751));
#4234=CARTESIAN_POINT('Ctrl Pts',(16.0418141788407,1.5,1.26289667008938));
#4235=CARTESIAN_POINT('Ctrl Pts',(16.0618970949743,1.5,1.26822275322431));
#4236=CARTESIAN_POINT('Ctrl Pts',(16.0882246094682,1.49999999999999,1.27520493300331));
#4237=CARTESIAN_POINT('Ctrl Pts',(16.1138379307147,1.49999999999999,1.28283870442167));
#4238=CARTESIAN_POINT('Ctrl Pts',(16.1389630519792,1.49999999999999,1.29112215414976));
#4239=CARTESIAN_POINT('Ctrl Pts',(16.1644211208015,1.49999999999999,1.29951537267571));
#4240=CARTESIAN_POINT('Ctrl Pts',(16.1893779380213,1.49999999999999,1.30857567974431));
#4241=CARTESIAN_POINT('Ctrl Pts',(16.2140509832687,1.5,1.31835164075651));
#4242=CARTESIAN_POINT('Ctrl Pts',(16.2308102903248,1.5,1.32499201816954));
#4243=CARTESIAN_POINT('Ctrl Pts',(16.2474383074032,1.5,1.33196362561461));
#4244=CARTESIAN_POINT('Ctrl Pts',(16.2639986895245,1.5,1.33929460616079));
#4245=CARTESIAN_POINT('Ctrl Pts',(16.2925242729341,1.50000000000001,1.35192236411413));
#4246=CARTESIAN_POINT('Ctrl Pts',(16.3205868967279,1.5,1.36552327695976));
#4247=CARTESIAN_POINT('Ctrl Pts',(16.348180133584,1.5,1.38003619580369));
#4248=CARTESIAN_POINT('Ctrl Pts',(16.376380791422,1.5,1.39486859334674));
#4249=CARTESIAN_POINT('Ctrl Pts',(16.4040926941819,1.49999999999999,1.41065437194904));
#4250=CARTESIAN_POINT('Ctrl Pts',(16.4312911408889,1.49999999999999,1.42737762082488));
#4251=CARTESIAN_POINT('Ctrl Pts',(16.4390157188017,1.49999999999999,1.43212715818957));
#4252=CARTESIAN_POINT('Ctrl Pts',(16.4466986927062,1.49999999999999,1.43695257148943));
#4253=CARTESIAN_POINT('Ctrl Pts',(16.4543389695688,1.49999999999999,1.44185406580663));
#4254=CARTESIAN_POINT('Ctrl Pts',(16.4764978585172,1.49999999999999,1.45606973759572));
#4255=CARTESIAN_POINT('Ctrl Pts',(16.4984000805429,1.49999999999999,1.47097635009296));
#4256=CARTESIAN_POINT('Ctrl Pts',(16.5198521810087,1.49999999999999,1.48643402849482));
#4257=CARTESIAN_POINT('Ctrl Pts',(16.5419826698061,1.49999999999999,1.50238053122786));
#4258=CARTESIAN_POINT('Ctrl Pts',(16.5636341493956,1.49999999999999,1.51891346464515));
#4259=CARTESIAN_POINT('Ctrl Pts',(16.5846293319728,1.49999999999999,1.53583491243833));
#4260=CARTESIAN_POINT('Ctrl Pts',(16.5989255129361,1.49999999999999,1.5473571785069));
#4261=CARTESIAN_POINT('Ctrl Pts',(16.6129181448062,1.49999999999999,1.55905863572717));
#4262=CARTESIAN_POINT('Ctrl Pts',(16.6265597698144,1.5,1.57086604116992));
#4263=CARTESIAN_POINT('Ctrl Pts',(16.6572577480919,1.5,1.59743644429841));
#4264=CARTESIAN_POINT('Ctrl Pts',(16.6863334374287,1.5,1.62473096009712));
#4265=CARTESIAN_POINT('Ctrl Pts',(16.7138746062607,1.5,1.65239273695287));
#4266=CARTESIAN_POINT('Ctrl Pts',(16.7417717673141,1.49999999999999,1.68041206498768));
#4267=CARTESIAN_POINT('Ctrl Pts',(16.7680945286679,1.49999999999999,1.70880833035569));
#4268=CARTESIAN_POINT('Ctrl Pts',(16.7929376483549,1.49999999999999,1.73726493227113));
#4269=CARTESIAN_POINT('Ctrl Pts',(16.8183752648702,1.49999999999998,1.76640250178618));
#4270=CARTESIAN_POINT('Ctrl Pts',(16.8422616279212,1.49999999999998,1.7956033909819));
#4271=CARTESIAN_POINT('Ctrl Pts',(16.8647014075051,1.49999999999997,1.82458300822481));
#4272=CARTESIAN_POINT('Ctrl Pts',(16.8820172700989,1.49999999999997,1.84694539678223));
#4273=CARTESIAN_POINT('Ctrl Pts',(16.8984718222692,1.49999999999997,1.8691771923285));
#4274=CARTESIAN_POINT('Ctrl Pts',(16.9141139993378,1.49999999999998,1.89116874693433));
#4275=CARTESIAN_POINT('Ctrl Pts',(16.9345229122745,1.49999999999998,1.91986192188849));
#4276=CARTESIAN_POINT('Ctrl Pts',(16.9538674058155,1.49999999999999,1.9485294650334));
#4277=CARTESIAN_POINT('Ctrl Pts',(16.9723861669818,1.49999999999999,1.97724358210273));
#4278=CARTESIAN_POINT('Ctrl Pts',(16.9925517880249,1.49999999999999,2.00851122458723));
#4279=CARTESIAN_POINT('Ctrl Pts',(17.0117380772993,1.5,2.03983422915842));
#4280=CARTESIAN_POINT('Ctrl Pts',(17.0302016163928,1.5,2.07134003671764));
#4281=CARTESIAN_POINT('Ctrl Pts',(17.0507711646618,1.50000000000001,2.10643949549775));
#4282=CARTESIAN_POINT('Ctrl Pts',(17.0704434160113,1.50000000000001,2.14176601350759));
#4283=CARTESIAN_POINT('Ctrl Pts',(17.0895152061429,1.50000000000001,2.17753420398472));
#4284=CARTESIAN_POINT('Ctrl Pts',(17.1041102362821,1.50000000000001,2.2049064545411));
#4285=CARTESIAN_POINT('Ctrl Pts',(17.1183522320751,1.50000000000002,2.23253828069445));
#4286=CARTESIAN_POINT('Ctrl Pts',(17.1323574194186,1.50000000000002,2.26053700349877));
#4287=CARTESIAN_POINT('Ctrl Pts',(17.1905958043563,1.50000000000002,2.3769653208395));
#4288=CARTESIAN_POINT('Ctrl Pts',(17.2430687017406,1.50000000000001,2.49654517074463));
#4289=CARTESIAN_POINT('Ctrl Pts',(17.2937552864049,1.49999999999999,2.61706719569844));
#4290=CARTESIAN_POINT('Ctrl Pts',(17.2989790764655,1.49999999999999,2.62948826845757));
#4291=CARTESIAN_POINT('Ctrl Pts',(17.3041839329455,1.49999999999998,2.64191931324455));
#4292=CARTESIAN_POINT('Ctrl Pts',(17.3093742528659,1.49999999999998,2.65435787846686));
#4293=CARTESIAN_POINT('Ctrl Pts',(17.4414703649819,1.49999999999992,2.97092528304739));
#4294=CARTESIAN_POINT('Ctrl Pts',(17.5736371531937,1.49999999999998,3.28766206239461));
#4295=CARTESIAN_POINT('Ctrl Pts',(17.7057705722715,1.50000000000001,3.6043188728468));
#4296=CARTESIAN_POINT('Origin',(1.14001967775083,0.,4.86953436266123));
#4297=CARTESIAN_POINT('',(12.2112288551483,0.,2.96506760632555));
#4298=CARTESIAN_POINT('',(12.2112288551483,0.,2.96506760632555));
#4299=CARTESIAN_POINT('',(15.5758189333363,0.,2.23621039387092));
#4300=CARTESIAN_POINT('Origin',(12.2112288551483,0.,2.96506760632555));
#4301=CARTESIAN_POINT('',(12.2112288551483,1.13559712679391,2.96506760632555));
#4302=CARTESIAN_POINT('',(12.2112288551483,0.,2.96506760632555));
#4303=CARTESIAN_POINT('',(12.2112288551483,1.13559712679391,2.96506760632555));
#4304=CARTESIAN_POINT('Origin',(15.5758189333363,0.,2.23621039387092));
#4305=CARTESIAN_POINT('Ctrl Pts',(15.5758189333363,0.500001553330218,2.23621039387092));
#4306=CARTESIAN_POINT('Ctrl Pts',(15.5730336227227,0.500001882640314,2.23681376417234));
#4307=CARTESIAN_POINT('Ctrl Pts',(15.5702580407276,0.500018346317171,2.23741502700341));
#4308=CARTESIAN_POINT('Ctrl Pts',(15.5643001119515,0.50008718504273,2.23870566843635));
#4309=CARTESIAN_POINT('Ctrl Pts',(15.5611274155881,0.500144191417668,2.23939295650823));
#4310=CARTESIAN_POINT('Ctrl Pts',(15.5510117219381,0.500388368687124,2.24158427732426));
#4311=CARTESIAN_POINT('Ctrl Pts',(15.5440683103694,0.500649781031692,2.24308839981268));
#4312=CARTESIAN_POINT('Ctrl Pts',(15.5152010219118,0.502094399985514,2.24934180094249));
#4313=CARTESIAN_POINT('Ctrl Pts',(15.4932093723954,0.504055639212508,2.25410576088748));
#4314=CARTESIAN_POINT('Ctrl Pts',(15.2021332613909,0.538654377367701,2.31716037317271));
#4315=CARTESIAN_POINT('Ctrl Pts',(14.857471604382,0.679244250275084,2.39182300033673));
#4316=CARTESIAN_POINT('Ctrl Pts',(13.758009643497,1.01645800356828,2.62999489093509));
#4317=CARTESIAN_POINT('Ctrl Pts',(13.1844003185397,1.10083856412948,2.75425350310206));
#4318=CARTESIAN_POINT('Ctrl Pts',(12.5183408466543,1.1300613879725,2.89853920766812));
#4319=CARTESIAN_POINT('Ctrl Pts',(12.4381215277557,1.13247032707045,2.91591678645149));
#4320=CARTESIAN_POINT('Ctrl Pts',(12.3317848486809,1.13439812345724,2.93895206079133));
#4321=CARTESIAN_POINT('Ctrl Pts',(12.3054859847343,1.13477708481274,2.94464907475779));
#4322=CARTESIAN_POINT('Ctrl Pts',(12.2563519030578,1.13530868818302,2.95529278735724));
#4323=CARTESIAN_POINT('Ctrl Pts',(12.2337962495623,1.13548464416554,2.96017892514812));
#4324=CARTESIAN_POINT('Ctrl Pts',(12.2112288551483,1.13559712679392,2.96506760632553));
#4325=CARTESIAN_POINT('Ctrl Pts',(-34.0397312276251,1.50001651647932,-1.36909522182877));
#4326=CARTESIAN_POINT('Ctrl Pts',(-33.1924498698387,1.50001651647932,-0.612825791490121));
#4327=CARTESIAN_POINT('Ctrl Pts',(-32.3451685120505,1.50001651647932,0.143443638845921));
#4328=CARTESIAN_POINT('Ctrl Pts',(-31.2860668148188,1.50001651647932,1.08878042677087));
#4329=CARTESIAN_POINT('Ctrl Pts',(-31.0742464753715,1.50001651647932,1.27784778435461));
#4330=CARTESIAN_POINT('Ctrl Pts',(-30.756515966202,1.50001651647932,1.56144882073196));
#4331=CARTESIAN_POINT('Ctrl Pts',(-30.6506057964787,1.50001651647932,1.65598249952408));
#4332=CARTESIAN_POINT('Ctrl Pts',(-30.4917405418936,1.50001651647932,1.79778301771254));
#4333=CARTESIAN_POINT('Ctrl Pts',(-30.4387854570318,1.50001651647932,1.84504985710868));
#4334=CARTESIAN_POINT('Ctrl Pts',(-30.3725916009548,1.50001651647932,1.90413340635381));
#4335=CARTESIAN_POINT('Ctrl Pts',(-30.3593528297393,1.50001651647932,1.91595011620282));
#4336=CARTESIAN_POINT('Ctrl Pts',(-30.3328752873086,1.50001651647932,1.9395835359009));
#4337=CARTESIAN_POINT('Ctrl Pts',(-30.3196192754619,1.50001651647932,1.95137367689095));
#4338=CARTESIAN_POINT('Ctrl Pts',(-30.279760622108,1.50001651647932,1.98660505148068));
#4339=CARTESIAN_POINT('Ctrl Pts',(-30.2530838382129,1.50001651647932,2.00993238371371));
#4340=CARTESIAN_POINT('Ctrl Pts',(-29.7978109883261,1.50001651647932,2.40378259345705));
#4341=CARTESIAN_POINT('Ctrl Pts',(-29.3426281831049,1.50001651647932,2.73347543301461));
#4342=CARTESIAN_POINT('Ctrl Pts',(-28.3829118941348,1.50001651647932,3.31707202741814));
#4343=CARTESIAN_POINT('Ctrl Pts',(-27.8783875922888,1.50001651647932,3.57098988537781));
#4344=CARTESIAN_POINT('Ctrl Pts',(-27.0888633012187,1.50001651647932,3.90159045490631));
#4345=CARTESIAN_POINT('Ctrl Pts',(-26.8200407752322,1.50001651647932,4.00340708499724));
#4346=CARTESIAN_POINT('Ctrl Pts',(-26.2812668399142,1.50001651647932,4.1889095609928));
#4347=CARTESIAN_POINT('Ctrl Pts',(-26.0101801979463,1.50001651647932,4.27310549979575));
#4348=CARTESIAN_POINT('Ctrl Pts',(-24.6474983424516,1.50001651647932,4.65759925751976));
#4349=CARTESIAN_POINT('Ctrl Pts',(-23.5345222531661,1.50001651647932,4.85027683035403));
#4350=CARTESIAN_POINT('Ctrl Pts',(-21.8492529263652,1.50001651647932,5.05973886640617));
#4351=CARTESIAN_POINT('Ctrl Pts',(-21.2847354172308,1.50001651647932,5.11600347268612));
#4352=CARTESIAN_POINT('Ctrl Pts',(-20.1530422384387,1.50001651647932,5.21376207945505));
#4353=CARTESIAN_POINT('Ctrl Pts',(-19.5870931764672,1.50001651647932,5.25457415792074));
#4354=CARTESIAN_POINT('Ctrl Pts',(-17.8889409412059,1.50001651647932,5.35299518486675));
#4355=CARTESIAN_POINT('Ctrl Pts',(-16.7564329002056,1.50001651647932,5.38660322444038));
#4356=CARTESIAN_POINT('Ctrl Pts',(-14.4906119904705,1.50001651647932,5.39045877557458));
#4357=CARTESIAN_POINT('Ctrl Pts',(-13.3572991273454,1.50001651647932,5.36070672866599));
#4358=CARTESIAN_POINT('Ctrl Pts',(-11.6567280104122,1.50001651647932,5.26869988662586));
#4359=CARTESIAN_POINT('Ctrl Pts',(-11.08998101943,1.50001651647932,5.22990018811796));
#4360=CARTESIAN_POINT('Ctrl Pts',(-9.9585090978714,1.50001651647932,5.13906450906196));
#4361=CARTESIAN_POINT('Ctrl Pts',(-9.39348094946301,1.50001651647932,5.08709034211947));
#4362=CARTESIAN_POINT('Ctrl Pts',(-6.57095080537902,1.50001651647932,4.80303784019359));
#4363=CARTESIAN_POINT('Ctrl Pts',(-4.32119839454725,1.50001651647932,4.49917594155329));
#4364=CARTESIAN_POINT('Ctrl Pts',(-0.941769866396083,1.50001651647932,4.08783925511307));
#4365=CARTESIAN_POINT('Ctrl Pts',(0.185432109304758,1.50001651647932,3.95808364226252));
#4366=CARTESIAN_POINT('Ctrl Pts',(2.44353563975074,1.50001651647932,3.73637424342037));
#4367=CARTESIAN_POINT('Ctrl Pts',(3.5742710607959,1.50001651647932,3.64270201570121));
#4368=CARTESIAN_POINT('Ctrl Pts',(5.83512987615239,1.50001651647932,3.44911395232651));
#4369=CARTESIAN_POINT('Ctrl Pts',(6.96588483332604,1.50001651647932,3.34948547984982));
#4370=CARTESIAN_POINT('Ctrl Pts',(9.21983034667651,1.50001651647932,3.09959443172648));
#4371=CARTESIAN_POINT('Ctrl Pts',(10.3405486815635,1.50001651647932,2.95006508649919));
#4372=CARTESIAN_POINT('Ctrl Pts',(11.5857377971987,1.50001651647932,2.72045164141356));
#4373=CARTESIAN_POINT('Ctrl Pts',(11.7239082995516,1.50001651647932,2.69421641700119));
#4374=CARTESIAN_POINT('Ctrl Pts',(11.9994569735669,1.50001651647932,2.63863200974361));
#4375=CARTESIAN_POINT('Ctrl Pts',(12.1368170203099,1.50001651647932,2.60921153318681));
#4376=CARTESIAN_POINT('Ctrl Pts',(12.5468187105572,1.50001651647932,2.51278085720776));
#4377=CARTESIAN_POINT('Ctrl Pts',(12.8173110539038,1.50001651647932,2.43732295077689));
#4378=CARTESIAN_POINT('Ctrl Pts',(13.3490272719293,1.50001651647932,2.24997621492956));
#4379=CARTESIAN_POINT('Ctrl Pts',(13.6102291757378,1.50001651647932,2.13800097705185));
#4380=CARTESIAN_POINT('Ctrl Pts',(13.9302791991952,1.50001651647932,1.97266934719546));
#4381=CARTESIAN_POINT('Ctrl Pts',(13.9939729118908,1.50001651647932,1.93835975838601));
#4382=CARTESIAN_POINT('Ctrl Pts',(14.0890439919513,1.50001651647932,1.88504992700688));
#4383=CARTESIAN_POINT('Ctrl Pts',(14.1206561581996,1.50001651647932,1.86697262234482));
#4384=CARTESIAN_POINT('Ctrl Pts',(14.1837255100384,1.50001651647932,1.8302088204661));
#4385=CARTESIAN_POINT('Ctrl Pts',(14.2151762379575,1.50001651647932,1.81149697580309));
#4386=CARTESIAN_POINT('Ctrl Pts',(14.3093533352867,1.50001651647932,1.75467275956207));
#4387=CARTESIAN_POINT('Ctrl Pts',(14.3719491491779,1.50001651647932,1.71604690764134));
#4388=CARTESIAN_POINT('Ctrl Pts',(14.4974115851479,1.50001651647932,1.6398591106154));
#4389=CARTESIAN_POINT('Ctrl Pts',(14.5602712714872,1.50001651647932,1.6022698894133));
#4390=CARTESIAN_POINT('Ctrl Pts',(14.7499431421768,1.50001651647932,1.49379697508882));
#4391=CARTESIAN_POINT('Ctrl Pts',(14.8776419496855,1.50001651647932,1.42729843352251));
#4392=CARTESIAN_POINT('Ctrl Pts',(15.1416347973429,1.50001651647932,1.31719971452458));
#4393=CARTESIAN_POINT('Ctrl Pts',(15.2777376799236,1.50001651647932,1.27361438637636));
#4394=CARTESIAN_POINT('Ctrl Pts',(15.5625910875211,1.50001651647932,1.22175349312147));
#4395=CARTESIAN_POINT('Ctrl Pts',(15.7059309495787,1.50001651647932,1.21455072070237));
#4396=CARTESIAN_POINT('Ctrl Pts',(15.920927592172,1.50001651647932,1.23677953415729));
#4397=CARTESIAN_POINT('Ctrl Pts',(15.9926752933312,1.50001651647932,1.24984772075882));
#4398=CARTESIAN_POINT('Ctrl Pts',(16.131127364388,1.50001651647932,1.28656585649914));
#4399=CARTESIAN_POINT('Ctrl Pts',(16.1984885496428,1.50001651647932,1.31027639396509));
#4400=CARTESIAN_POINT('Ctrl Pts',(16.3295222008884,1.50001651647932,1.36828261273081));
#4401=CARTESIAN_POINT('Ctrl Pts',(16.3936981208766,1.50001651647932,1.40293130074928));
#4402=CARTESIAN_POINT('Ctrl Pts',(16.5149976550397,1.50001651647932,1.48074902752459));
#4403=CARTESIAN_POINT('Ctrl Pts',(16.5723029825951,1.50001651647932,1.52388264495703));
#4404=CARTESIAN_POINT('Ctrl Pts',(16.7351057716355,1.50001651647932,1.66479536878992));
#4405=CARTESIAN_POINT('Ctrl Pts',(16.8313021633667,1.50001651647932,1.77471393776967));
#4406=CARTESIAN_POINT('Ctrl Pts',(16.9969527535348,1.50001651647932,2.00760440967715));
#4407=CARTESIAN_POINT('Ctrl Pts',(17.0680061729772,1.50001651647932,2.13185112918205));
#4408=CARTESIAN_POINT('Ctrl Pts',(17.1967382089781,1.50001651647932,2.38920810011174));
#4409=CARTESIAN_POINT('Ctrl Pts',(17.2539932137629,1.50001651647932,2.52159471797806));
#4410=CARTESIAN_POINT('Ctrl Pts',(17.309389495544,1.50001651647932,2.65435151805373));
#4411=CARTESIAN_POINT('Ctrl Pts',(17.4439154500122,1.50001651647932,2.97674202276166));
#4412=CARTESIAN_POINT('Ctrl Pts',(17.5784414044805,1.50001651647932,3.29913252746959));
#4413=CARTESIAN_POINT('Ctrl Pts',(17.7129673589487,1.50001651647932,3.62152303217752));
#4414=CARTESIAN_POINT('Ctrl Pts',(-34.7056444293428,0.499999999999992,-0.623043855628343));
#4415=CARTESIAN_POINT('Ctrl Pts',(-33.8583630715561,0.499999999999992,0.133225574709989));
#4416=CARTESIAN_POINT('Ctrl Pts',(-33.0110817137697,0.499999999999992,0.889495005047924));
#4417=CARTESIAN_POINT('Ctrl Pts',(-31.9519800165362,0.499999999999992,1.83483179297088));
#4418=CARTESIAN_POINT('Ctrl Pts',(-31.7401596770896,0.499999999999992,2.02389915055542));
#4419=CARTESIAN_POINT('Ctrl Pts',(-31.4224291679196,0.499999999999992,2.30750018693225));
#4420=CARTESIAN_POINT('Ctrl Pts',(-31.3165189981963,0.499999999999992,2.40203386572442));
#4421=CARTESIAN_POINT('Ctrl Pts',(-31.1576537436113,0.499999999999992,2.54383438391295));
#4422=CARTESIAN_POINT('Ctrl Pts',(-31.1046986587496,0.499999999999992,2.59110122330912));
#4423=CARTESIAN_POINT('Ctrl Pts',(-31.0385048026725,0.499999999999992,2.6501847725542));
#4424=CARTESIAN_POINT('Ctrl Pts',(-31.0252660314571,0.499999999999992,2.66200148240322));
#4425=CARTESIAN_POINT('Ctrl Pts',(-30.9987884890263,0.499999999999992,2.68563490210131));
#4426=CARTESIAN_POINT('Ctrl Pts',(-30.9832388632707,0.499999999999992,2.69946808101334));
#4427=CARTESIAN_POINT('Ctrl Pts',(-30.9393834899522,0.499999999999992,2.73823218750993));
#4428=CARTESIAN_POINT('Ctrl Pts',(-30.9100301799479,0.499999999999992,2.7639000016916));
#4429=CARTESIAN_POINT('Ctrl Pts',(-30.4090631337961,0.499999999999992,3.19727962452407));
#4430=CARTESIAN_POINT('Ctrl Pts',(-29.9079156984876,0.499999999999992,3.56012215843322));
#4431=CARTESIAN_POINT('Ctrl Pts',(-28.8567836899866,0.499999999999992,4.19930799510662));
#4432=CARTESIAN_POINT('Ctrl Pts',(-28.3069163147731,0.499999999999992,4.475698392225));
#4433=CARTESIAN_POINT('Ctrl Pts',(-27.4539677767877,0.499999999999992,4.8328568415799));
#4434=CARTESIAN_POINT('Ctrl Pts',(-27.164747699717,0.499999999999993,4.94235355832733));
#4435=CARTESIAN_POINT('Ctrl Pts',(-26.5876684807393,0.499999999999993,5.14104472765234));
#4436=CARTESIAN_POINT('Ctrl Pts',(-26.2985764248276,0.499999999999992,5.2307936706632));
#4437=CARTESIAN_POINT('Ctrl Pts',(-24.851719466111,0.499999999999992,5.63903823819463));
#4438=CARTESIAN_POINT('Ctrl Pts',(-23.6903478434334,0.499999999999992,5.83862031478634));
#4439=CARTESIAN_POINT('Ctrl Pts',(-21.9563545557512,0.499999999999992,6.05413824694173));
#4440=CARTESIAN_POINT('Ctrl Pts',(-21.3802100145193,0.499999999999992,6.11149674921549));
#4441=CARTESIAN_POINT('Ctrl Pts',(-20.2296946994093,0.499999999999992,6.21088126116752));
#4442=CARTESIAN_POINT('Ctrl Pts',(-19.6543438808625,0.499999999999992,6.25237114523089));
#4443=CARTESIAN_POINT('Ctrl Pts',(-17.9280242560943,0.499999999999992,6.35242468975165));
#4444=CARTESIAN_POINT('Ctrl Pts',(-16.7767888220963,0.499999999999992,6.38658655078378));
#4445=CARTESIAN_POINT('Ctrl Pts',(-14.4736593465745,0.499999999999992,6.39050558666034));
#4446=CARTESIAN_POINT('Ctrl Pts',(-13.3217653084983,0.499999999999992,6.36026329011945));
#4447=CARTESIAN_POINT('Ctrl Pts',(-11.593456856115,0.499999999999992,6.26675576127116));
#4448=CARTESIAN_POINT('Ctrl Pts',(-11.0176742635534,0.499999999999931,6.22732924297478));
#4449=CARTESIAN_POINT('Ctrl Pts',(-9.87076616810186,0.500000000000054,6.13525433228844));
#4450=CARTESIAN_POINT('Ctrl Pts',(-9.29903474634851,0.499999999999992,6.08265330862635));
#4451=CARTESIAN_POINT('Ctrl Pts',(-6.44806855419954,0.499999999999992,5.79573907165103));
#4452=CARTESIAN_POINT('Ctrl Pts',(-4.19197936980058,0.499999999999992,5.49084470148195));
#4453=CARTESIAN_POINT('Ctrl Pts',(-0.825137262501205,0.499999999999992,
5.08104000571533));
#4454=CARTESIAN_POINT('Ctrl Pts',(0.293273733998886,0.499999999999993,4.95232040469897));
#4455=CARTESIAN_POINT('Ctrl Pts',(2.5311253192372,0.499999999999993,4.73259942190914));
#4456=CARTESIAN_POINT('Ctrl Pts',(3.65773355433088,0.499999999999869,4.6392312433788));
#4457=CARTESIAN_POINT('Ctrl Pts',(5.92229763284814,0.500000000000115,4.44532591472657));
#4458=CARTESIAN_POINT('Ctrl Pts',(7.0608573913797,0.500000000000238,4.34509976949567));
#4459=CARTESIAN_POINT('Ctrl Pts',(9.34524764280534,0.499999999999746,4.09183336732117));
#4460=CARTESIAN_POINT('Ctrl Pts',(10.4885105555597,0.500000000000114,3.93965728369929));
#4461=CARTESIAN_POINT('Ctrl Pts',(11.7712568966956,0.499999999999977,3.70311827029293));
#4462=CARTESIAN_POINT('Ctrl Pts',(11.9138517815751,0.499999999999993,3.67606050201731));
#4463=CARTESIAN_POINT('Ctrl Pts',(12.2049990926623,0.499999999999993,3.61732950098476));
#4464=CARTESIAN_POINT('Ctrl Pts',(12.3527978405267,0.500000000000007,3.58571697834473));
#4465=CARTESIAN_POINT('Ctrl Pts',(12.8017143158579,0.499999999999962,3.48013371530843));
#4466=CARTESIAN_POINT('Ctrl Pts',(13.1087015369894,0.499999999999961,3.39492840425144));
#4467=CARTESIAN_POINT('Ctrl Pts',(13.7222853032534,0.500000000000023,3.17873617812773));
#4468=CARTESIAN_POINT('Ctrl Pts',(14.0281358746551,0.499999999999961,3.04768383691634));
#4469=CARTESIAN_POINT('Ctrl Pts',(14.3995116112702,0.5,2.8558383396111));
#4470=CARTESIAN_POINT('Ctrl Pts',(14.473269524189,0.5,2.81610352931213));
#4471=CARTESIAN_POINT('Ctrl Pts',(14.5830463690884,0.499999999999988,2.75454763752365));
#4472=CARTESIAN_POINT('Ctrl Pts',(14.6194957575626,0.499999999999988,2.73370357088325));
#4473=CARTESIAN_POINT('Ctrl Pts',(14.6920997332583,0.499999999999996,2.69138193423077));
#4474=CARTESIAN_POINT('Ctrl Pts',(14.7287241088115,0.499999999999992,2.66958471801292));
#4475=CARTESIAN_POINT('Ctrl Pts',(14.8321427204664,0.499999999999992,2.60718437024267));
#4476=CARTESIAN_POINT('Ctrl Pts',(14.8947429371819,0.499999999999992,2.56853667987705));
#4477=CARTESIAN_POINT('Ctrl Pts',(15.0127324953208,0.499999999999992,2.49688681601923));
#4478=CARTESIAN_POINT('Ctrl Pts',(15.0679261119592,0.499999999999992,2.46394621747195));
#4479=CARTESIAN_POINT('Ctrl Pts',(15.2239960512198,0.499999999999992,2.37469015503045));
#4480=CARTESIAN_POINT('Ctrl Pts',(15.3151397369363,0.500000000000023,2.32833861119067));
#4481=CARTESIAN_POINT('Ctrl Pts',(15.4739865129508,0.499999999999961,2.26209124628497));
#4482=CARTESIAN_POINT('Ctrl Pts',(15.5412102426098,0.499999999999976,2.24210104315146));
#4483=CARTESIAN_POINT('Ctrl Pts',(15.6573592971275,0.500000000000008,2.22095473893486));
#4484=CARTESIAN_POINT('Ctrl Pts',(15.7044313152833,0.499999999999992,2.21974296559136));
#4485=CARTESIAN_POINT('Ctrl Pts',(15.767410117571,0.499999999999992,2.22625443129171));
#4486=CARTESIAN_POINT('Ctrl Pts',(15.787122043338,0.499999999999985,2.2299203684438));
#4487=CARTESIAN_POINT('Ctrl Pts',(15.8239859664479,0.5,2.23969685326193));
#4488=CARTESIAN_POINT('Ctrl Pts',(15.84126845336,0.5,2.24576246549322));
#4489=CARTESIAN_POINT('Ctrl Pts',(15.8771446395265,0.499999999999984,2.26164420179718));
#4490=CARTESIAN_POINT('Ctrl Pts',(15.8955951643463,0.5,2.27149430071215));
#4491=CARTESIAN_POINT('Ctrl Pts',(15.9331444677752,0.499999999999985,2.2955834436242));
#4492=CARTESIAN_POINT('Ctrl Pts',(15.952275277354,0.499999999999992,2.3098037266637));
#4493=CARTESIAN_POINT('Ctrl Pts',(16.0117937275615,0.499999999999992,2.36131947594947));
#4494=CARTESIAN_POINT('Ctrl Pts',(16.0546868722937,0.499999999999992,2.40816900698943));
#4495=CARTESIAN_POINT('Ctrl Pts',(16.1437612346005,0.499999999999992,2.53339991517352));
#4496=CARTESIAN_POINT('Ctrl Pts',(16.190212071248,0.499999999999992,2.6123539981433));
#4497=CARTESIAN_POINT('Ctrl Pts',(16.2857972214586,0.499999999999992,2.80344480969631));
#4498=CARTESIAN_POINT('Ctrl Pts',(16.3343667769681,0.499999999999992,2.91452246837103));
#4499=CARTESIAN_POINT('Ctrl Pts',(16.386497303637,0.499999999999992,3.03945284932728));
#4500=CARTESIAN_POINT('Ctrl Pts',(16.5130926026644,0.499999999999992,3.34283744843543));
#4501=CARTESIAN_POINT('Ctrl Pts',(16.6396879016917,0.499999999999992,3.64622204754358));
#4502=CARTESIAN_POINT('Ctrl Pts',(16.766283200719,0.499999999999992,3.94960664665173));
#4503=CARTESIAN_POINT('Ctrl Pts',(-34.7123034513764,0.489999999999992,-0.615583465185726));
#4504=CARTESIAN_POINT('Ctrl Pts',(-33.8650220935896,0.489999999999992,0.140685965152536));
#4505=CARTESIAN_POINT('Ctrl Pts',(-33.0177407358033,0.489999999999992,0.896955395490548));
#4506=CARTESIAN_POINT('Ctrl Pts',(-31.9586390385697,0.489999999999992,1.84229218341346));
#4507=CARTESIAN_POINT('Ctrl Pts',(-31.7468186991232,0.489999999999992,2.03135954099803));
#4508=CARTESIAN_POINT('Ctrl Pts',(-31.4290881899532,0.489999999999992,2.31496057737484));
#4509=CARTESIAN_POINT('Ctrl Pts',(-31.3231780202299,0.489999999999992,2.40949425616707));
#4510=CARTESIAN_POINT('Ctrl Pts',(-31.1643127656449,0.489999999999992,2.55129477435557));
#4511=CARTESIAN_POINT('Ctrl Pts',(-31.1113576807832,0.489999999999992,2.59856161375176));
#4512=CARTESIAN_POINT('Ctrl Pts',(-31.0451638247061,0.489999999999992,2.65764516299682));
#4513=CARTESIAN_POINT('Ctrl Pts',(-31.0319250534907,0.489999999999992,2.66946187284586));
#4514=CARTESIAN_POINT('Ctrl Pts',(-31.0054475110599,0.489999999999992,2.69309529254392));
#4515=CARTESIAN_POINT('Ctrl Pts',(-30.9898749495441,0.489999999999992,2.70694890149773));
#4516=CARTESIAN_POINT('Ctrl Pts',(-30.945979609686,0.489999999999992,2.74574833473001));
#4517=CARTESIAN_POINT('Ctrl Pts',(-30.9165995348626,0.489999999999991,2.7714395533445));
#4518=CARTESIAN_POINT('Ctrl Pts',(-30.4151755542951,0.489999999999991,3.20521446377914));
#4519=CARTESIAN_POINT('Ctrl Pts',(-29.9135684802773,0.489999999999992,3.5683884891567));
#4520=CARTESIAN_POINT('Ctrl Pts',(-28.8615223296795,0.489999999999992,4.2081302090716));
#4521=CARTESIAN_POINT('Ctrl Pts',(-28.3112015312213,0.489999999999992,4.48474532786999));
#4522=CARTESIAN_POINT('Ctrl Pts',(-27.457618761242,0.489999999999992,4.84216935163674));
#4523=CARTESIAN_POINT('Ctrl Pts',(-27.1681947120293,0.489999999999992,4.9517428679823));
#4524=CARTESIAN_POINT('Ctrl Pts',(-26.5907324465417,0.489999999999992,5.15056592206242));
#4525=CARTESIAN_POINT('Ctrl Pts',(-26.3014603394644,0.489999999999992,5.24037039419811));
#4526=CARTESIAN_POINT('Ctrl Pts',(-24.8537616436179,0.489999999999992,5.64885246590485));
#4527=CARTESIAN_POINT('Ctrl Pts',(-23.6919060735996,0.489999999999992,5.8485035863938));
#4528=CARTESIAN_POINT('Ctrl Pts',(-21.957425554356,0.489999999999992,6.06408207651008));
#4529=CARTESIAN_POINT('Ctrl Pts',(-21.3811647447234,0.489999999999992,6.12145151756312));
#4530=CARTESIAN_POINT('Ctrl Pts',(-20.230461211359,0.489999999999992,6.22085228829844));
#4531=CARTESIAN_POINT('Ctrl Pts',(-19.6550163767992,0.489999999999992,6.26234895030581));
#4532=CARTESIAN_POINT('Ctrl Pts',(-17.9284150827881,0.489999999999992,6.36241881973267));
#4533=CARTESIAN_POINT('Ctrl Pts',(-16.7769923779532,0.489999999999992,6.3965862188879));
#4534=CARTESIAN_POINT('Ctrl Pts',(-14.4734898229355,0.489999999999992,6.40050588960137));
#4535=CARTESIAN_POINT('Ctrl Pts',(-13.3214099761787,0.489999999999992,6.37025869064512));
#4536=CARTESIAN_POINT('Ctrl Pts',(-11.592824155022,0.489999999999992,6.27673615517661));
#4537=CARTESIAN_POINT('Ctrl Pts',(-11.016951207937,0.48999999999993,6.2373033687859));
#4538=CARTESIAN_POINT('Ctrl Pts',(-9.86988875329596,0.490000000000055,6.14521606598797));
#4539=CARTESIAN_POINT('Ctrl Pts',(-9.29809029991629,0.489999999999992,6.0926087738622));
#4540=CARTESIAN_POINT('Ctrl Pts',(-6.44683975198322,0.489999999999992,5.80566592000903));
#4541=CARTESIAN_POINT('Ctrl Pts',(-4.19068720089519,0.489999999999992,5.50076122529517));
#4542=CARTESIAN_POINT('Ctrl Pts',(-0.823970955725548,0.489999999999992,
5.09097184918228));
#4543=CARTESIAN_POINT('Ctrl Pts',(0.294352132434478,0.489999999999992,4.96226260811314));
#4544=CARTESIAN_POINT('Ctrl Pts',(2.53200120156563,0.489999999999992,4.7425615091555));
#4545=CARTESIAN_POINT('Ctrl Pts',(3.65856816548137,0.489999999999868,4.64919637106674));
#4546=CARTESIAN_POINT('Ctrl Pts',(5.92316929601833,0.490000000000116,4.45528786981418));
#4547=CARTESIAN_POINT('Ctrl Pts',(7.06180710127438,0.49000000000024,4.35505574795442));
#4548=CARTESIAN_POINT('Ctrl Pts',(9.34650179505245,0.489999999999744,4.1017555927969));
#4549=CARTESIAN_POINT('Ctrl Pts',(10.489990149862,0.490000000000115,3.9495530422282));
#4550=CARTESIAN_POINT('Ctrl Pts',(11.7731120570498,0.489999999999977,3.7129447742825));
#4551=CARTESIAN_POINT('Ctrl Pts',(11.9157511850239,0.489999999999992,3.68587878070408));
#4552=CARTESIAN_POINT('Ctrl Pts',(12.2070544799055,0.489999999999992,3.62711631425347));
#4553=CARTESIAN_POINT('Ctrl Pts',(12.3549576130571,0.490000000000008,3.59548187151465));
#4554=CARTESIAN_POINT('Ctrl Pts',(12.8042632298119,0.489999999999962,3.48980708411944));
#4555=CARTESIAN_POINT('Ctrl Pts',(13.1116153936936,0.489999999999961,3.40450430062607));
#4556=CARTESIAN_POINT('Ctrl Pts',(13.7260178219185,0.490000000000023,3.1880236243638));
#4557=CARTESIAN_POINT('Ctrl Pts',(14.0323148726219,0.48999999999996,3.05678051526989));
#4558=CARTESIAN_POINT('Ctrl Pts',(14.4042038578915,0.49,2.86466988366926));
#4559=CARTESIAN_POINT('Ctrl Pts',(14.4780624111504,0.49,2.82488082205141));
#4560=CARTESIAN_POINT('Ctrl Pts',(14.5879863112693,0.489999999999988,2.7632424710208));
#4561=CARTESIAN_POINT('Ctrl Pts',(14.6244840711669,0.489999999999988,2.74237073721757));
#4562=CARTESIAN_POINT('Ctrl Pts',(14.6971833915264,0.489999999999997,2.69999352313528));
#4563=CARTESIAN_POINT('Ctrl Pts',(14.7338595027015,0.489999999999992,2.67816545371149));
#4564=CARTESIAN_POINT('Ctrl Pts',(14.8373705279732,0.489999999999992,2.61570934554691));
#4565=CARTESIAN_POINT('Ctrl Pts',(14.8999707887162,0.489999999999992,2.57706143680043));
#4566=CARTESIAN_POINT('Ctrl Pts',(15.0178856193111,0.489999999999992,2.50545695152482));
#4567=CARTESIAN_POINT('Ctrl Pts',(15.0730025765186,0.489999999999992,2.47256283843628));
#4568=CARTESIAN_POINT('Ctrl Pts',(15.2287365020147,0.489999999999992,2.38349894133971));
#4569=CARTESIAN_POINT('Ctrl Pts',(15.3195146425508,0.490000000000023,2.33734886414972));
#4570=CARTESIAN_POINT('Ctrl Pts',(15.477309975215,0.489999999999961,2.27154000554233));
#4571=CARTESIAN_POINT('Ctrl Pts',(15.543844924721,0.489999999999977,2.25178574976194));
#4572=CARTESIAN_POINT('Ctrl Pts',(15.6583069635714,0.490000000000008,2.23094658636282));
#4573=CARTESIAN_POINT('Ctrl Pts',(15.704416319188,0.489999999999992,2.22979472202062));
#4574=CARTESIAN_POINT('Ctrl Pts',(15.7658749681803,0.489999999999992,2.23614901683935));
#4575=CARTESIAN_POINT('Ctrl Pts',(15.7850665447876,0.489999999999984,2.23972093304985));
#4576=CARTESIAN_POINT('Ctrl Pts',(15.8209146031966,0.49,2.24922800580848));
#4577=CARTESIAN_POINT('Ctrl Pts',(15.8376963113963,0.49,2.25511717170168));
#4578=CARTESIAN_POINT('Ctrl Pts',(15.8726209386285,0.489999999999984,2.2705776701384));
#4579=CARTESIAN_POINT('Ctrl Pts',(15.8906142170488,0.49,2.28017978725815));
#4580=CARTESIAN_POINT('Ctrl Pts',(15.9273260320027,0.489999999999984,2.30373165320545));
#4581=CARTESIAN_POINT('Ctrl Pts',(15.9460751027066,0.489999999999992,2.31766280767642));
#4582=CARTESIAN_POINT('Ctrl Pts',(16.0045607265845,0.489999999999992,2.36828460198171));
#4583=CARTESIAN_POINT('Ctrl Pts',(16.0469208476503,0.489999999999992,2.41450345305888));
#4584=CARTESIAN_POINT('Ctrl Pts',(16.135229460326,0.489999999999992,2.53865778338701));
#4585=CARTESIAN_POINT('Ctrl Pts',(16.181434275209,0.489999999999992,2.61715894747207));
#4586=CARTESIAN_POINT('Ctrl Pts',(16.2766879620364,0.489999999999992,2.80758710837596));
#4587=CARTESIAN_POINT('Ctrl Pts',(16.3251706644875,0.489999999999992,2.91845168097819));
#4588=CARTESIAN_POINT('Ctrl Pts',(16.3772685341448,0.489999999999992,3.04330379903588));
#4589=CARTESIAN_POINT('Ctrl Pts',(16.5037845279275,0.489999999999992,3.34649834222707));
#4590=CARTESIAN_POINT('Ctrl Pts',(16.6303005217103,0.489999999999992,3.64969288541828));
#4591=CARTESIAN_POINT('Ctrl Pts',(16.756816515493,0.489999999999992,3.95288742860948));
#4592=CARTESIAN_POINT('',(0.,0.,0.));
#4593=CARTESIAN_POINT('',(0.,0.,0.));
#4594=CARTESIAN_POINT('Origin',(0.,0.,-0.451382872428838));
#4595=CARTESIAN_POINT('',(-2.33486982377251E-16,0.,-1.45138287242884));
#4596=CARTESIAN_POINT('Origin',(0.,0.,-0.451382872428838));
#4597=CARTESIAN_POINT('',(-2.33486982377251E-16,1.2,-1.45138287242884));
#4598=CARTESIAN_POINT('',(-2.3348698237725E-16,0.,-1.45138287242884));
#4599=CARTESIAN_POINT('Origin',(0.,1.2,-0.451382872428838));
#4600=CARTESIAN_POINT('Ctrl Pts',(-7.09134809128677,1.2,-7.28017474573539));
#4601=CARTESIAN_POINT('Ctrl Pts',(-7.09134809128677,0.912000000000082,-7.28017474573539));
#4602=CARTESIAN_POINT('Ctrl Pts',(-26.0573343465012,1.2,-19.1299473575062));
#4603=CARTESIAN_POINT('Ctrl Pts',(-26.0573343465012,0.912000000000082,-19.1299473575062));
#4604=CARTESIAN_POINT('Ctrl Pts',(-47.6352267379569,1.2,-23.4630266781973));
#4605=CARTESIAN_POINT('Ctrl Pts',(-47.6352267379569,0.912000000000082,-23.4630266781973));
#4606=CARTESIAN_POINT('',(-7.09134809128677,1.2,-7.28017474573539));
#4607=CARTESIAN_POINT('',(-7.09134823816015,1.00000000000006,-7.28017467283774));
#4608=CARTESIAN_POINT('',(-7.09134809128677,1.2,-7.28017474573539));
#4609=CARTESIAN_POINT('',(-47.6352266725888,1.00000007481202,-23.463026510487));
#4610=CARTESIAN_POINT('Ctrl Pts',(-7.09134831553042,1.00000000000006,-7.28017453553405));
#4611=CARTESIAN_POINT('Ctrl Pts',(-7.11068751337854,1.00000000000006,-7.29225607297566));
#4612=CARTESIAN_POINT('Ctrl Pts',(-7.13014127538947,1.00000000000006,-7.3044055075262));
#4613=CARTESIAN_POINT('Ctrl Pts',(-7.20288303224859,1.00000000000006,-7.34979888829056));
#4614=CARTESIAN_POINT('Ctrl Pts',(-7.2562856468552,1.00000000000006,-7.38307141655157));
#4615=CARTESIAN_POINT('Ctrl Pts',(-7.36308604485071,1.00000000000006,-7.44950314916467));
#4616=CARTESIAN_POINT('Ctrl Pts',(-7.41650933220709,1.00000000000006,-7.48267908965507));
#4617=CARTESIAN_POINT('Ctrl Pts',(-7.57688126501097,1.00000000000006,-7.58210746819504));
#4618=CARTESIAN_POINT('Ctrl Pts',(-7.68386634925554,1.00000000000006,-7.64821950621151));
#4619=CARTESIAN_POINT('Ctrl Pts',(-8.00522827087396,1.00000000000006,-7.84615547748184));
#4620=CARTESIAN_POINT('Ctrl Pts',(-8.43461654073609,1.00000000000006,-8.10888740557686));
#4621=CARTESIAN_POINT('Ctrl Pts',(-8.86481189078967,1.00000000000006,-8.36863733500345));
#4622=CARTESIAN_POINT('Ctrl Pts',(-9.51221899491459,1.00000000000005,-8.75693190854638));
#4623=CARTESIAN_POINT('Ctrl Pts',(-9.94498238629759,1.00000000000006,-9.01300707260298));
#4624=CARTESIAN_POINT('Ctrl Pts',(-11.2495773841444,1.00000000000006,-9.77452717708374));
#4625=CARTESIAN_POINT('Ctrl Pts',(-12.1240421591257,1.00000000000006,-10.2710077251322));
#4626=CARTESIAN_POINT('Ctrl Pts',(-13.8850801361361,1.00000000000006,-11.2430286125482));
#4627=CARTESIAN_POINT('Ctrl Pts',(-14.7716680498301,1.00000000000006,-11.7184360575102));
#4628=CARTESIAN_POINT('Ctrl Pts',(-16.1094164672201,1.00000000000006,-12.4149117109426));
#4629=CARTESIAN_POINT('Ctrl Pts',(-16.5574356159811,1.00000000000006,-12.6446827728682));
#4630=CARTESIAN_POINT('Ctrl Pts',(-17.4559246536095,1.00000000000006,-13.0985360950426));
#4631=CARTESIAN_POINT('Ctrl Pts',(-17.906495383924,1.00000000000006,-13.3226581958257));
#4632=CARTESIAN_POINT('Ctrl Pts',(-19.2630950583786,1.00000000000006,-13.9870499958456));
#4633=CARTESIAN_POINT('Ctrl Pts',(-20.1719150319432,1.00000000000006,-14.4182572383939));
#4634=CARTESIAN_POINT('Ctrl Pts',(-21.9998979114302,1.00000000000006,-15.2579388305516));
#4635=CARTESIAN_POINT('Ctrl Pts',(-22.9191119697774,1.00000000000006,-15.6663622503542));
#4636=CARTESIAN_POINT('Ctrl Pts',(-24.768006788053,1.00000000000006,-16.4603187472532));
#4637=CARTESIAN_POINT('Ctrl Pts',(-25.6976797513383,1.00000000000006,-16.8457952774682));
#4638=CARTESIAN_POINT('Ctrl Pts',(-27.620212900096,1.00000000000006,-17.6147290858774));
#4639=CARTESIAN_POINT('Ctrl Pts',(-28.6120762515168,1.00000000000006,-17.9961739561557));
#4640=CARTESIAN_POINT('Ctrl Pts',(-30.4984832918179,1.00000000000006,-18.6929702060858));
#4641=CARTESIAN_POINT('Ctrl Pts',(-31.3921908423818,1.00000000000006,-19.0110399067431));
#4642=CARTESIAN_POINT('Ctrl Pts',(-33.2952368599222,1.00000000000006,-19.6629165069278));
#4643=CARTESIAN_POINT('Ctrl Pts',(-34.3055473016782,1.00000000000006,-19.9939988746763));
#4644=CARTESIAN_POINT('Ctrl Pts',(-36.2228941614421,1.00000000000006,-20.5941180293612));
#4645=CARTESIAN_POINT('Ctrl Pts',(-37.1288738936713,1.00000000000006,-20.8659549929327));
#4646=CARTESIAN_POINT('Ctrl Pts',(-39.003851405174,1.00000000000006,-21.4044110917491));
#4647=CARTESIAN_POINT('Ctrl Pts',(-39.9735095225768,1.00000000000006,-21.6697762014278));
#4648=CARTESIAN_POINT('Ctrl Pts',(-41.4346591386383,1.00000000000006,-22.0500145741695));
#4649=CARTESIAN_POINT('Ctrl Pts',(-41.9223778391297,1.00000000000006,-22.1736882842118));
#4650=CARTESIAN_POINT('Ctrl Pts',(-42.8996532716617,1.00000000000006,-22.4150132014848));
#4651=CARTESIAN_POINT('Ctrl Pts',(-43.3893152843367,1.00000000000006,-22.5326978063825));
#4652=CARTESIAN_POINT('Ctrl Pts',(-44.3696193969244,1.00000000000006,-22.7618534517681));
#4653=CARTESIAN_POINT('Ctrl Pts',(-44.8604283639025,1.00000000000006,-22.8733785049591));
#4654=CARTESIAN_POINT('Ctrl Pts',(-45.5979342111895,1.00000000000006,-23.0361575203374));
#4655=CARTESIAN_POINT('Ctrl Pts',(-46.0894060993012,1.00000000000006,-23.1430409487816));
#4656=CARTESIAN_POINT('Ctrl Pts',(-46.5820249421721,1.00000000000006,-23.2469929425543));
#4657=CARTESIAN_POINT('Ctrl Pts',(-46.951626660381,1.00000000000006,-23.3237965794452));
#4658=CARTESIAN_POINT('Ctrl Pts',(-47.074831674522,1.00000000000006,-23.34920099103));
#4659=CARTESIAN_POINT('Ctrl Pts',(-47.2597235085411,1.00000000000006,-23.3870284915049));
#4660=CARTESIAN_POINT('Ctrl Pts',(-47.3213549739448,1.00000000000006,-23.3995884807167));
#4661=CARTESIAN_POINT('Ctrl Pts',(-47.4446371365223,1.00000000000006,-23.4246136938071));
#4662=CARTESIAN_POINT('Ctrl Pts',(-47.5063193313214,1.00000000000006,-23.4370845030402));
#4663=CARTESIAN_POINT('Ctrl Pts',(-47.5903801898929,1.00000000000006,-23.4540147689754));
#4664=CARTESIAN_POINT('Ctrl Pts',(-47.6128719552537,1.00000000000006,-23.4585359892155));
#4665=CARTESIAN_POINT('Ctrl Pts',(-47.6352267041176,1.00000000000006,-23.4630263535246));
#4666=CARTESIAN_POINT('',(-47.6352267379569,1.2,-23.4630266781973));
#4667=CARTESIAN_POINT('',(-47.6352267379569,1.2,-23.4630266781973));
#4668=CARTESIAN_POINT('Ctrl Pts',(-7.09134809128677,1.2,-7.28017474573539));
#4669=CARTESIAN_POINT('Ctrl Pts',(-26.0573343465012,1.2,-19.1299473575062));
#4670=CARTESIAN_POINT('Ctrl Pts',(-47.6352267379569,1.2,-23.4630266781973));
#4671=CARTESIAN_POINT('Ctrl Pts',(-47.6352267379569,1.2,-23.4630266781973));
#4672=CARTESIAN_POINT('Ctrl Pts',(-47.6352267379569,-0.5280000000419,-23.4630266781973));
#4673=CARTESIAN_POINT('Ctrl Pts',(-41.2879795894165,1.2,-16.3973366595173));
#4674=CARTESIAN_POINT('Ctrl Pts',(-41.2879795894165,-0.5280000000419,-16.3973366595173));
#4675=CARTESIAN_POINT('Ctrl Pts',(-28.9390638541746,1.2,-7.40052527015664));
#4676=CARTESIAN_POINT('Ctrl Pts',(-28.9390638541746,-0.5280000000419,-7.40052527015664));
#4677=CARTESIAN_POINT('Ctrl Pts',(-11.4361348672924,1.2,0.292821829763132));
#4678=CARTESIAN_POINT('Ctrl Pts',(-11.4361348672924,-0.5280000000419,0.292821829763132));
#4679=CARTESIAN_POINT('Ctrl Pts',(-2.50014102937161,1.2,3.94559933269074));
#4680=CARTESIAN_POINT('Ctrl Pts',(-2.50014102937161,-0.5280000000419,3.94559933269074));
#4681=CARTESIAN_POINT('Ctrl Pts',(1.18077271965353,1.2,5.54861712757117));
#4682=CARTESIAN_POINT('Ctrl Pts',(1.18077271965353,-0.5280000000419,5.54861712757117));
#4683=CARTESIAN_POINT('',(-46.4732177923012,0.,-22.2016498092846));
#4684=CARTESIAN_POINT('Ctrl Pts',(-47.6352265853192,1.00000017512283,-23.4630265082826));
#4685=CARTESIAN_POINT('Ctrl Pts',(-47.5497337833158,0.923530724722877,-23.3678568040681));
#4686=CARTESIAN_POINT('Ctrl Pts',(-47.4664431491314,0.849654487371893,-23.275672245252));
#4687=CARTESIAN_POINT('Ctrl Pts',(-47.3838551040137,0.777007709588356,-23.1847477783321));
#4688=CARTESIAN_POINT('Ctrl Pts',(-47.3000081267036,0.7032535394808,-23.0924373028402));
#4689=CARTESIAN_POINT('Ctrl Pts',(-47.2168852312997,0.630766597197125,-23.0014256885189));
#4690=CARTESIAN_POINT('Ctrl Pts',(-47.1328800183873,0.558119808566171,-22.9099457634324));
#4691=CARTESIAN_POINT('Ctrl Pts',(-47.1080751876962,0.536668862490658,-22.8829338200692));
#4692=CARTESIAN_POINT('Ctrl Pts',(-47.0831931883918,0.515203979624482,-22.8558812926668));
#4693=CARTESIAN_POINT('Ctrl Pts',(-47.0581920598092,0.493688420180458,-22.8287433089684));
#4694=CARTESIAN_POINT('Ctrl Pts',(-46.8651256765308,0.327538670886058,-22.6191754750683));
#4695=CARTESIAN_POINT('Ctrl Pts',(-46.6701360902887,0.162956146341853,-22.4101382936785));
#4696=CARTESIAN_POINT('Ctrl Pts',(-46.4732177923012,0.,-22.2016498092846));
#4697=CARTESIAN_POINT('',(1.18077271965353,0.,5.54861712757117));
#4698=CARTESIAN_POINT('Ctrl Pts',(-46.4732177923012,0.,-22.2016498092846));
#4699=CARTESIAN_POINT('Ctrl Pts',(-40.3530658599041,0.,-15.7219005239919));
#4700=CARTESIAN_POINT('Ctrl Pts',(-25.1069939231375,0.,-4.7997213617563));
#4701=CARTESIAN_POINT('Ctrl Pts',(-7.64469421946831,0.,1.70517457060066));
#4702=CARTESIAN_POINT('Ctrl Pts',(1.18077271965353,0.,5.54861712757117));
#4703=CARTESIAN_POINT('',(1.18077271965353,1.2,5.54861712757117));
#4704=CARTESIAN_POINT('',(1.18077271965353,1.2,5.54861712757117));
#4705=CARTESIAN_POINT('Ctrl Pts',(-47.6352267379569,1.2,-23.4630266781973));
#4706=CARTESIAN_POINT('Ctrl Pts',(-41.2879795894165,1.2,-16.3973366595173));
#4707=CARTESIAN_POINT('Ctrl Pts',(-25.6436006166727,1.2,-4.99961317195811));
#4708=CARTESIAN_POINT('Ctrl Pts',(-7.64469421946831,1.2,1.70517457060066));
#4709=CARTESIAN_POINT('Ctrl Pts',(1.18077271965353,1.2,5.54861712757117));
#4710=CARTESIAN_POINT('Ctrl Pts',(4.63072594339218,1.2,4.37702154953648));
#4711=CARTESIAN_POINT('Ctrl Pts',(4.63072594339218,-0.528,4.37702154953648));
#4712=CARTESIAN_POINT('Ctrl Pts',(4.7840847941358,1.2,4.31192383490808));
#4713=CARTESIAN_POINT('Ctrl Pts',(4.7840847941358,-0.528,4.31192383490808));
#4714=CARTESIAN_POINT('Ctrl Pts',(6.57703737715603,1.2,3.59239489692552));
#4715=CARTESIAN_POINT('Ctrl Pts',(6.57703737715603,-0.528,3.59239489692552));
#4716=CARTESIAN_POINT('Ctrl Pts',(9.67706435206833,1.2,3.76607425470487));
#4717=CARTESIAN_POINT('Ctrl Pts',(9.67706435206833,-0.528,3.76607425470487));
#4718=CARTESIAN_POINT('Ctrl Pts',(14.6739773919611,1.2,5.78899007926008));
#4719=CARTESIAN_POINT('Ctrl Pts',(14.6739773919611,-0.528,5.78899007926008));
#4720=CARTESIAN_POINT('Ctrl Pts',(21.529136784602,1.2,8.35971201308491));
#4721=CARTESIAN_POINT('Ctrl Pts',(21.529136784602,-0.528,8.35971201308491));
#4722=CARTESIAN_POINT('Ctrl Pts',(29.5112752479747,1.2,12.6039811673409));
#4723=CARTESIAN_POINT('Ctrl Pts',(29.5112752479747,-0.528,12.6039811673409));
#4724=CARTESIAN_POINT('Ctrl Pts',(36.9335047542113,1.2,17.1028493432964));
#4725=CARTESIAN_POINT('Ctrl Pts',(36.9335047542113,-0.528,17.1028493432964));
#4726=CARTESIAN_POINT('Ctrl Pts',(41.8538494170237,1.2,20.3434433890621));
#4727=CARTESIAN_POINT('Ctrl Pts',(41.8538494170237,-0.528,20.3434433890621));
#4728=CARTESIAN_POINT('Ctrl Pts',(48.2654669907203,1.2,23.135880733102));
#4729=CARTESIAN_POINT('Ctrl Pts',(48.2654669907203,-0.528,23.135880733102));
#4730=CARTESIAN_POINT('Ctrl Pts',(48.9333109271159,1.2,18.4504184980571));
#4731=CARTESIAN_POINT('Ctrl Pts',(48.9333109271159,-0.528,18.4504184980571));
#4732=CARTESIAN_POINT('Ctrl Pts',(42.3375494192901,1.2,14.5257061310277));
#4733=CARTESIAN_POINT('Ctrl Pts',(42.3375494192901,-0.528,14.5257061310277));
#4734=CARTESIAN_POINT('',(42.3375494192901,1.2,14.5257061310277));
#4735=CARTESIAN_POINT('',(42.3375494192901,0.,14.5257061310277));
#4736=CARTESIAN_POINT('',(42.3375494192901,1.2,14.5257061310277));
#4737=CARTESIAN_POINT('',(4.63072594277028,1.2,4.37702154980046));
#4738=CARTESIAN_POINT('Ctrl Pts',(4.63072594339218,1.2,4.37702154953648));
#4739=CARTESIAN_POINT('Ctrl Pts',(4.7840847941358,1.2,4.31192383490808));
#4740=CARTESIAN_POINT('Ctrl Pts',(6.57703737715603,1.2,3.59239489692552));
#4741=CARTESIAN_POINT('Ctrl Pts',(9.67706435206833,1.2,3.76607425470487));
#4742=CARTESIAN_POINT('Ctrl Pts',(14.6739773919611,1.2,5.78899007926008));
#4743=CARTESIAN_POINT('Ctrl Pts',(21.529136784602,1.2,8.35971201308491));
#4744=CARTESIAN_POINT('Ctrl Pts',(29.5112752479747,1.2,12.6039811673409));
#4745=CARTESIAN_POINT('Ctrl Pts',(36.9335047542113,1.2,17.1028493432964));
#4746=CARTESIAN_POINT('Ctrl Pts',(41.8538494170237,1.2,20.3434433890621));
#4747=CARTESIAN_POINT('Ctrl Pts',(48.2654669907203,1.2,23.135880733102));
#4748=CARTESIAN_POINT('Ctrl Pts',(48.9333109271159,1.2,18.4504184980571));
#4749=CARTESIAN_POINT('Ctrl Pts',(42.3375494192901,1.2,14.5257061310277));
#4750=CARTESIAN_POINT('',(4.63072594277028,0.,4.37702154980046));
#4751=CARTESIAN_POINT('',(4.63072594277027,1.2,4.37702154980048));
#4752=CARTESIAN_POINT('Ctrl Pts',(4.63072594339218,4.16333634234434E-16,
4.37702154953648));
#4753=CARTESIAN_POINT('Ctrl Pts',(4.7840847941358,4.16333634234434E-16,
4.31192383490808));
#4754=CARTESIAN_POINT('Ctrl Pts',(6.57703737715603,4.16333634234434E-16,
3.59239489692552));
#4755=CARTESIAN_POINT('Ctrl Pts',(9.67706435206833,4.16333634234434E-16,
3.76607425470487));
#4756=CARTESIAN_POINT('Ctrl Pts',(14.6739773919611,4.16333634234434E-16,
5.78899007926008));
#4757=CARTESIAN_POINT('Ctrl Pts',(21.529136784602,4.16333634234434E-16,
8.35971201308491));
#4758=CARTESIAN_POINT('Ctrl Pts',(29.5112752479747,4.16333634234434E-16,
12.6039811673409));
#4759=CARTESIAN_POINT('Ctrl Pts',(36.9335047542113,4.16333634234434E-16,
17.1028493432964));
#4760=CARTESIAN_POINT('Ctrl Pts',(41.8538494170237,4.16333634234434E-16,
20.3434433890621));
#4761=CARTESIAN_POINT('Ctrl Pts',(48.2654669907203,4.16333634234434E-16,
23.135880733102));
#4762=CARTESIAN_POINT('Ctrl Pts',(48.9333109271159,4.16333634234434E-16,
18.4504184980571));
#4763=CARTESIAN_POINT('Ctrl Pts',(42.3375494192901,4.16333634234434E-16,
14.5257061310277));
#4764=CARTESIAN_POINT('Ctrl Pts',(42.3375494192901,1.2,14.5257061310277));
#4765=CARTESIAN_POINT('Ctrl Pts',(42.3375494192901,-0.528,14.5257061310277));
#4766=CARTESIAN_POINT('Ctrl Pts',(20.9640318338388,1.2,0.869135776253969));
#4767=CARTESIAN_POINT('Ctrl Pts',(20.9640318338388,-0.528,0.869135776253969));
#4768=CARTESIAN_POINT('Ctrl Pts',(-2.47626210225015,1.2,-8.83090725784708));
#4769=CARTESIAN_POINT('Ctrl Pts',(-2.47626210225015,-0.528,-8.83090725784708));
#4770=CARTESIAN_POINT('',(-2.47626210225015,0.,-8.83090725784708));
#4771=CARTESIAN_POINT('Ctrl Pts',(42.3375494192901,0.,14.5257061310277));
#4772=CARTESIAN_POINT('Ctrl Pts',(20.9640318338388,0.,0.869135776253969));
#4773=CARTESIAN_POINT('Ctrl Pts',(-2.47626210225015,0.,-8.83090725784708));
#4774=CARTESIAN_POINT('',(-2.47626210225015,1.2,-8.83090725784708));
#4775=CARTESIAN_POINT('',(-2.47626210225015,1.2,-8.83090725784708));
#4776=CARTESIAN_POINT('Ctrl Pts',(42.3375494192901,1.2,14.5257061310277));
#4777=CARTESIAN_POINT('Ctrl Pts',(20.9640318338388,1.2,0.869135776253969));
#4778=CARTESIAN_POINT('Ctrl Pts',(-2.47626210225015,1.2,-8.83090725784708));
#4779=CARTESIAN_POINT('Origin',(-2.47626210225015,1.2,-8.83090725784708));
#4780=CARTESIAN_POINT('',(-8.32185266851751,0.,-6.86670824505761));
#4781=CARTESIAN_POINT('',(-2.47626210225015,0.,-8.83090725784708));
#4782=CARTESIAN_POINT('Ctrl Pts',(-8.32185266851834,1.14311338172968E-12,
-6.86670824505734));
#4783=CARTESIAN_POINT('Ctrl Pts',(-8.11928072190117,0.164182972460768,-6.93477521161165));
#4784=CARTESIAN_POINT('Ctrl Pts',(-7.91680514284801,0.328508227719272,-7.00280979716715));
#4785=CARTESIAN_POINT('Ctrl Pts',(-7.51215815602449,0.657345458539218,-7.13877676287178));
#4786=CARTESIAN_POINT('Ctrl Pts',(-7.37869817804401,0.765866874721603,-7.18362115541202));
#4787=CARTESIAN_POINT('Ctrl Pts',(-7.09134844131163,1.00000001188238,-7.28017462812221));
#4788=CARTESIAN_POINT('',(-2.47626210225015,1.2,-8.83090725784708));
#4789=CARTESIAN_POINT('Origin',(-26.7103108805615,1.2,-17.2507740347362));
#4790=CARTESIAN_POINT('',(1.18077271965353,1.2,5.54861712757117));
#4791=CARTESIAN_POINT('Origin',(-26.7103108805615,0.,-17.2507740347362));
#4792=CARTESIAN_POINT('Ctrl Pts',(-46.4732177922936,0.,-22.2016498093203));
#4793=CARTESIAN_POINT('Ctrl Pts',(-46.415282761538,5.07841822769624E-16,
-22.1893264214989));
#4794=CARTESIAN_POINT('Ctrl Pts',(-46.3573586444288,1.28814513242496E-15,
-22.176961010912));
#4795=CARTESIAN_POINT('Ctrl Pts',(-46.2994454089906,1.77635683940025E-15,
-22.1645535547065));
#4796=CARTESIAN_POINT('Ctrl Pts',(-46.0553963173232,3.8337038815267E-15,
-22.1122679520467));
#4797=CARTESIAN_POINT('Ctrl Pts',(-45.8115404634548,5.56211880942695E-15,
-22.0592357000739));
#4798=CARTESIAN_POINT('Ctrl Pts',(-45.5678754638484,7.32747196252603E-15,
-22.0054550434754));
#4799=CARTESIAN_POINT('Ctrl Pts',(-45.0803415951789,1.08596553031322E-14,
-21.8978487331172));
#4800=CARTESIAN_POINT('Ctrl Pts',(-44.5935547144433,1.37433652042168E-14,
-21.7872420837894));
#4801=CARTESIAN_POINT('Ctrl Pts',(-44.1075470623437,1.62092561595273E-14,
-21.6736330559672));
#4802=CARTESIAN_POINT('Ctrl Pts',(-43.6213030745586,1.86763462277054E-14,
-21.559968782374));
#4803=CARTESIAN_POINT('Ctrl Pts',(-43.1356693881152,2.06773659315811E-14,
-21.443256509246));
#4804=CARTESIAN_POINT('Ctrl Pts',(-42.65115708627,2.26485497023532E-14,
-21.3236127657438));
#4805=CARTESIAN_POINT('Ctrl Pts',(-42.1664508837015,2.46205223363956E-14,
-21.2039211410871));
#4806=CARTESIAN_POINT('Ctrl Pts',(-41.6827582533232,2.48053267803675E-14,
-21.0812721899324));
#4807=CARTESIAN_POINT('Ctrl Pts',(-41.2001345714453,2.62012633811537E-14,
-20.9556779035789));
#4808=CARTESIAN_POINT('Ctrl Pts',(-40.2344744599496,2.87722289092885E-14,
-20.7043819205649));
#4809=CARTESIAN_POINT('Ctrl Pts',(-39.2727950142657,2.70692054571062E-14,
-20.4412269998355));
#4810=CARTESIAN_POINT('Ctrl Pts',(-38.3151477577178,2.62012633811537E-14,
-20.1662098332526));
#4811=CARTESIAN_POINT('Ctrl Pts',(-37.0552642848644,2.50593963007545E-14,
-19.8043964614086));
#4812=CARTESIAN_POINT('Ctrl Pts',(-35.8021293334856,2.23739275243883E-14,
-19.4219998183265));
#4813=CARTESIAN_POINT('Ctrl Pts',(-34.5554354702551,1.95399252334028E-14,
-19.018867339076));
#4814=CARTESIAN_POINT('Ctrl Pts',(-33.9064143565704,1.80645611706375E-14,
-18.8089990639827));
#4815=CARTESIAN_POINT('Ctrl Pts',(-33.2591391506989,1.64907532665174E-14,
-18.5935101896125));
#4816=CARTESIAN_POINT('Ctrl Pts',(-32.6135681765606,1.50990331349021E-14,
-18.3723738593228));
#4817=CARTESIAN_POINT('Ctrl Pts',(-31.3769595799164,1.24331557212291E-14,
-17.94878125987));
#4818=CARTESIAN_POINT('Ctrl Pts',(-30.1465313472377,1.0222160868584E-14,
-17.504445383288));
#4819=CARTESIAN_POINT('Ctrl Pts',(-28.9220387964689,9.76996261670138E-15,
-17.0391634027186));
#4820=CARTESIAN_POINT('Ctrl Pts',(-28.280905786778,9.53319578130951E-15,
-16.7955460476191));
#4821=CARTESIAN_POINT('Ctrl Pts',(-27.6414002959298,9.73942422296218E-15,
-16.5461855556373));
#4822=CARTESIAN_POINT('Ctrl Pts',(-27.003489002828,1.06581410364015E-14,
-16.2910473999339));
#4823=CARTESIAN_POINT('Ctrl Pts',(-26.9214424596597,1.07763040780476E-14,
-16.2582321732211));
#4824=CARTESIAN_POINT('Ctrl Pts',(-26.8394331456511,1.09599753714691E-14,
-16.2253257263837));
#4825=CARTESIAN_POINT('Ctrl Pts',(-26.7574608858174,1.11022302462516E-14,
-16.1923280234092));
#4826=CARTESIAN_POINT('Ctrl Pts',(-26.6728122570399,1.1249129698721E-14,
-16.158252955633));
#4827=CARTESIAN_POINT('Ctrl Pts',(-26.5882109329397,1.1627230561039E-14,
-16.1240837088094));
#4828=CARTESIAN_POINT('Ctrl Pts',(-26.5036601420706,1.17683640610267E-14,
-16.0898217001875));
#4829=CARTESIAN_POINT('Ctrl Pts',(-25.7442601358659,1.3035966405898E-14,
-15.7820946015686));
#4830=CARTESIAN_POINT('Ctrl Pts',(-24.9888454631677,1.38814835013908E-14,
-15.4668487724091));
#4831=CARTESIAN_POINT('Ctrl Pts',(-24.237230782582,1.46549439250521E-14,
-15.1440887362585));
#4832=CARTESIAN_POINT('Ctrl Pts',(-23.3199064620055,1.55989303531444E-14,
-14.7501693005172));
#4833=CARTESIAN_POINT('Ctrl Pts',(-22.4082668273739,1.50548750441534E-14,
-14.3450675510963));
#4834=CARTESIAN_POINT('Ctrl Pts',(-21.5020580029957,1.62092561595273E-14,
-13.9288016897425));
#4835=CARTESIAN_POINT('Ctrl Pts',(-20.5952669744745,1.73643789201489E-14,
-13.5122683936621));
#4836=CARTESIAN_POINT('Ctrl Pts',(-19.6938847201665,1.57933555484948E-14,
-13.0845414602457));
#4837=CARTESIAN_POINT('Ctrl Pts',(-18.7977536862311,1.62092561595273E-14,
-12.645663195712));
#4838=CARTESIAN_POINT('Ctrl Pts',(-18.3495978945471,1.63062227585341E-14,
-12.4261798515952));
#4839=CARTESIAN_POINT('Ctrl Pts',(-17.9027032335625,1.57814290351876E-14,
-12.2038797705404));
#4840=CARTESIAN_POINT('Ctrl Pts',(-17.4571099588515,1.55431223447522E-14,
-11.9787974606056));
#4841=CARTESIAN_POINT('Ctrl Pts',(-17.0115235519992,1.53048193273002E-14,
-11.7537186198289));
#4842=CARTESIAN_POINT('Ctrl Pts',(-16.5671420195394,1.50389305983309E-14,
-11.5258063384921));
#4843=CARTESIAN_POINT('Ctrl Pts',(-16.1243005352796,1.46549439250521E-14,
-11.2952485538549));
#4844=CARTESIAN_POINT('Ctrl Pts',(-15.2388368853048,1.38871607490214E-14,
-10.8342471690002));
#4845=CARTESIAN_POINT('Ctrl Pts',(-14.359372072549,1.41875053432936E-14,
-10.3626017246681));
#4846=CARTESIAN_POINT('Ctrl Pts',(-13.4855627416189,1.22124532708767E-14,
-9.88029473784141));
#4847=CARTESIAN_POINT('Ctrl Pts',(-12.612368072651,1.02387905054168E-14,
-9.39832701926059));
#4848=CARTESIAN_POINT('Ctrl Pts',(-11.7448449913689,9.99403333149777E-15,
-8.90572622764085));
#4849=CARTESIAN_POINT('Ctrl Pts',(-10.8827350786316,8.65973959207622E-15,
-8.40249416572321));
#4850=CARTESIAN_POINT('Ctrl Pts',(-10.4520277880869,7.99313080727245E-15,
-8.15108107476871));
#4851=CARTESIAN_POINT('Ctrl Pts',(-10.0226717933981,4.28796303457655E-15,
-7.89701412660226));
#4852=CARTESIAN_POINT('Ctrl Pts',(-9.59463597909433,5.32907051820075E-15,
-7.64029160545447));
#4853=CARTESIAN_POINT('Ctrl Pts',(-9.3807251925437,5.84936371158235E-15,
-7.51199459247366));
#4854=CARTESIAN_POINT('Ctrl Pts',(-9.16714413194284,4.59352397126425E-15,
-7.38303433113536));
#4855=CARTESIAN_POINT('Ctrl Pts',(-8.95388898144895,4.66293670342566E-15,
-7.25341048871357));
#4856=CARTESIAN_POINT('Ctrl Pts',(-8.74289238468451,4.73161429561619E-15,
-7.12515947321788));
#4857=CARTESIAN_POINT('Ctrl Pts',(-8.53221483130022,4.37413988992977E-15,
-6.99625885790051));
#4858=CARTESIAN_POINT('Ctrl Pts',(-8.32185266851846,3.99680288865056E-15,
-6.86670824505608));
#4859=CARTESIAN_POINT('',(-16.8843114964558,0.,11.6834750258843));
#4860=CARTESIAN_POINT('Origin',(1.18077271965353,0.,5.54861712757117));
#4861=CARTESIAN_POINT('Ctrl Pts',(-5.24383419181389,1.00000000000006,-6.12586516693238));
#4862=CARTESIAN_POINT('Ctrl Pts',(-5.45552849279514,1.00000000000006,-6.25812980617024));
#4863=CARTESIAN_POINT('Ctrl Pts',(-5.66722279377639,1.00000000000006,-6.39039444540812));
#4864=CARTESIAN_POINT('Ctrl Pts',(-5.98476424524831,1.00000000000006,-6.58879140426484));
#4865=CARTESIAN_POINT('Ctrl Pts',(-6.09061139573891,1.00000000000006,-6.65492372388378));
#4866=CARTESIAN_POINT('Ctrl Pts',(-6.30230569672019,1.00000000000006,-6.78718836312159));
#4867=CARTESIAN_POINT('Ctrl Pts',(-6.40815284721083,1.00000000000006,-6.85332068274051));
#4868=CARTESIAN_POINT('Ctrl Pts',(-6.6198471481921,1.00000000000006,-6.98558532197835));
#4869=CARTESIAN_POINT('Ctrl Pts',(-6.72563063914494,1.00000000000006,-7.05168172755663));
#4870=CARTESIAN_POINT('Ctrl Pts',(-6.88449685418767,1.00000000000006,-7.15093407804603));
#4871=CARTESIAN_POINT('Ctrl Pts',(-6.93738368631082,1.00000000000006,-7.18398126018817));
#4872=CARTESIAN_POINT('Ctrl Pts',(-7.01677641920857,1.00000000000006,-7.23358203087279));
#4873=CARTESIAN_POINT('Ctrl Pts',(-7.04327503493536,1.00000000000006,-7.25013843752416));
#4874=CARTESIAN_POINT('Ctrl Pts',(-7.09612004061923,1.00000000000006,-7.2831569231934));
#4875=CARTESIAN_POINT('Ctrl Pts',(-7.12287909314553,1.00000000000006,-7.29987365377378));
#4876=CARTESIAN_POINT('Ctrl Pts',(-7.20287196849749,1.00000000000006,-7.34979198412591));
#4877=CARTESIAN_POINT('Ctrl Pts',(-7.25627459447878,1.00000000000006,-7.38306454177835));
#4878=CARTESIAN_POINT('Ctrl Pts',(-7.36307503586608,1.00000000000006,-7.44949630138193));
#4879=CARTESIAN_POINT('Ctrl Pts',(-7.41649833999293,1.00000000000006,-7.48267227463444));
#4880=CARTESIAN_POINT('Ctrl Pts',(-7.57683755810601,1.00000000000006,-7.58208037051894));
#4881=CARTESIAN_POINT('Ctrl Pts',(-7.68382277781079,1.00000000000006,-7.64819266931624));
#4882=CARTESIAN_POINT('Ctrl Pts',(-8.00505610385903,1.00000000000006,-7.84604943490794));
#4883=CARTESIAN_POINT('Ctrl Pts',(-8.21958187689062,1.00000000000006,-7.97731377158191));
#4884=CARTESIAN_POINT('Ctrl Pts',(-8.64937624226859,1.00000000000006,-8.23855762413463));
#4885=CARTESIAN_POINT('Ctrl Pts',(-8.86464483463895,1.00000000000006,-8.36853713993857));
#4886=CARTESIAN_POINT('Ctrl Pts',(-9.51156841532699,1.00000000000005,-8.75654171121627));
#4887=CARTESIAN_POINT('Ctrl Pts',(-9.94434120352226,1.00000000000006,-9.01263280045349));
#4888=CARTESIAN_POINT('Ctrl Pts',(-11.2471595199954,1.00000000000006,-9.77311581787846));
#4889=CARTESIAN_POINT('Ctrl Pts',(-12.1217049333607,1.00000000000006,-10.2697176721681));
#4890=CARTESIAN_POINT('Ctrl Pts',(-13.8829505118507,1.00000000000006,-11.2418531471041));
#4891=CARTESIAN_POINT('Ctrl Pts',(-14.7696264087533,1.00000000000006,-11.7173731122773));
#4892=CARTESIAN_POINT('Ctrl Pts',(-16.1089470909339,1.00000000000006,-12.4146673382703));
#4893=CARTESIAN_POINT('Ctrl Pts',(-16.5569782215825,1.00000000000006,-12.6444517294623));
#4894=CARTESIAN_POINT('Ctrl Pts',(-17.4554954883835,1.00000000000006,-13.0983193110247));
#4895=CARTESIAN_POINT('Ctrl Pts',(-17.9060788716974,1.00000000000006,-13.3224542098502));
#4896=CARTESIAN_POINT('Ctrl Pts',(-19.2616031097108,1.00000000000006,-13.9863193171645));
#4897=CARTESIAN_POINT('Ctrl Pts',(-20.1705291712439,1.00000000000006,-14.4176206450584));
#4898=CARTESIAN_POINT('Ctrl Pts',(-21.9987526788008,1.00000000000006,-15.2574127694115));
#4899=CARTESIAN_POINT('Ctrl Pts',(-22.9180793896471,1.00000000000006,-15.6659188375137));
#4900=CARTESIAN_POINT('Ctrl Pts',(-24.7672228950628,1.00000000000006,-16.4599821261938));
#4901=CARTESIAN_POINT('Ctrl Pts',(-25.6970148613833,1.00000000000006,-16.8455293489637));
#4902=CARTESIAN_POINT('Ctrl Pts',(-28.5023646567929,1.00000000000006,-17.9675533325283));
#4903=CARTESIAN_POINT('Ctrl Pts',(-30.3883028921554,1.00000000000006,-18.6671643210093));
#4904=CARTESIAN_POINT('Ctrl Pts',(-34.1907153053487,1.00000000000006,-19.9696570897424));
#4905=CARTESIAN_POINT('Ctrl Pts',(-36.1073577041579,1.00000000000006,-20.5725959425394));
#4906=CARTESIAN_POINT('Ctrl Pts',(-39.0050100165848,1.00000000000006,-21.4047438218093));
#4907=CARTESIAN_POINT('Ctrl Pts',(-39.9748094572256,1.00000000000006,-21.6701144864535));
#4908=CARTESIAN_POINT('Ctrl Pts',(-41.4350320957616,1.00000000000006,-22.0501116296716));
#4909=CARTESIAN_POINT('Ctrl Pts',(-41.922768748648,1.00000000000006,-22.173784814017));
#4910=CARTESIAN_POINT('Ctrl Pts',(-42.900075718841,1.00000000000006,-22.4151175190879));
#4911=CARTESIAN_POINT('Ctrl Pts',(-43.3897554961037,1.00000000000006,-22.5328007101756));
#4912=CARTESIAN_POINT('Ctrl Pts',(-44.370090732942,1.00000000000006,-22.7619636311583));
#4913=CARTESIAN_POINT('Ctrl Pts',(-44.8609173199214,1.00000000000006,-22.8734864251602));
#4914=CARTESIAN_POINT('Ctrl Pts',(-45.5980622108449,1.00000000000006,-23.0361857718529));
#4915=CARTESIAN_POINT('Ctrl Pts',(-45.8439323102181,1.00000000000006,-23.0896558259346));
#4916=CARTESIAN_POINT('Ctrl Pts',(-46.3359817814183,1.00000000000006,-23.19507356367));
#4917=CARTESIAN_POINT('Ctrl Pts',(-46.5821611532186,1.00000000000006,-23.2470212473572));
#4918=CARTESIAN_POINT('Ctrl Pts',(-46.9516614198392,1.00000000000006,-23.3238038024982));
#4919=CARTESIAN_POINT('Ctrl Pts',(-47.0748667102372,1.00000000000006,-23.349208159078));
#4920=CARTESIAN_POINT('Ctrl Pts',(-47.2597323553301,1.00000000000006,-23.3870303014924));
#4921=CARTESIAN_POINT('Ctrl Pts',(-47.321363855279,1.00000000000006,-23.3995902835508));
#4922=CARTESIAN_POINT('Ctrl Pts',(-47.444646076246,1.00000000000006,-23.4246155084937));
#4923=CARTESIAN_POINT('Ctrl Pts',(-47.5063283010135,1.00000000000006,-23.4370863095799));
#4924=CARTESIAN_POINT('Ctrl Pts',(-47.5987715311571,1.00000000000006,-23.4557048259362));
#4925=CARTESIAN_POINT('Ctrl Pts',(-47.6297134045,1.00000000000006,-23.4619201822993));
#4926=CARTESIAN_POINT('Ctrl Pts',(-47.6907845360928,1.00000000000006,-23.4741826558094));
#4927=CARTESIAN_POINT('Ctrl Pts',(-47.7214121565107,1.00000000000006,-23.4803327329731));
#4928=CARTESIAN_POINT('Ctrl Pts',(-47.813167153602,1.00000000000006,-23.498760940644));
#4929=CARTESIAN_POINT('Ctrl Pts',(-47.8743280692006,1.00000000000006,-23.5110408686088));
#4930=CARTESIAN_POINT('Ctrl Pts',(-47.9966589828603,1.00000000000006,-23.5356062683543));
#4931=CARTESIAN_POINT('Ctrl Pts',(-48.05782443969,1.00000000000006,-23.5478889682269));
#4932=CARTESIAN_POINT('Ctrl Pts',(-48.1801553533496,1.00000000000006,-23.5724543679724));
#4933=CARTESIAN_POINT('Ctrl Pts',(-48.2413208101794,1.00000000000006,-23.584737067845));
#4934=CARTESIAN_POINT('Ctrl Pts',(-48.4248171806689,1.00000000000006,-23.6215851674632));
#4935=CARTESIAN_POINT('Ctrl Pts',(-48.5471480943282,1.00000000000006,-23.6461505672086));
#4936=CARTESIAN_POINT('Ctrl Pts',(-48.7918099216474,1.00000000000006,-23.6952813666994));
#4937=CARTESIAN_POINT('Ctrl Pts',(-48.914140835307,1.00000000000006,-23.7198467664448));
#4938=CARTESIAN_POINT('Ctrl Pts',(-49.2811335762858,1.00000000000006,-23.793542965681));
#4939=CARTESIAN_POINT('Ctrl Pts',(-49.525795403605,1.00000000000006,-23.8426737651719));
#4940=CARTESIAN_POINT('Ctrl Pts',(-49.770457230924,1.00000000000006,-23.8918045646627));
#4941=CARTESIAN_POINT('Ctrl Pts',(-5.77370550858122,0.,-5.27778711175859));
#4942=CARTESIAN_POINT('Ctrl Pts',(-5.9853998095625,0.,-5.41005175099646));
#4943=CARTESIAN_POINT('Ctrl Pts',(-6.19709411054381,0.,-5.54231639023431));
#4944=CARTESIAN_POINT('Ctrl Pts',(-6.51463556201566,0.,-5.74071334909106));
#4945=CARTESIAN_POINT('Ctrl Pts',(-6.62048271250629,0.,-5.80684566871));
#4946=CARTESIAN_POINT('Ctrl Pts',(-6.83217701348755,0.,-5.93911030794779));
#4947=CARTESIAN_POINT('Ctrl Pts',(-6.93802416397819,0.,-6.00524262756673));
#4948=CARTESIAN_POINT('Ctrl Pts',(-7.14971846495949,0.,-6.13750726680458));
#4949=CARTESIAN_POINT('Ctrl Pts',(-7.25556400272244,0.,-6.20364240870763));
#4950=CARTESIAN_POINT('Ctrl Pts',(-7.41433714754994,0.,-6.30283665470982));
#4951=CARTESIAN_POINT('Ctrl Pts',(-7.46725906024219,0.,-6.33590572399238));
#4952=CARTESIAN_POINT('Ctrl Pts',(-7.54664570739394,0.,-6.38550271620998));
#4953=CARTESIAN_POINT('Ctrl Pts',(-7.57310736259635,0.,-6.40203602780547));
#4954=CARTESIAN_POINT('Ctrl Pts',(-7.62603034649297,0.,-6.43510322256449));
#4955=CARTESIAN_POINT('Ctrl Pts',(-7.65249300217831,0.,-6.45163478324257));
#4956=CARTESIAN_POINT('Ctrl Pts',(-7.73190363272615,-8.67361737988404E-16,
-6.50118980170777));
#4957=CARTESIAN_POINT('Ctrl Pts',(-7.78486602535483,8.67361737988404E-16,
-6.53418802672631));
#4958=CARTESIAN_POINT('Ctrl Pts',(-7.8908369143435,-8.67361737988404E-16,
-6.60010379009612));
#4959=CARTESIAN_POINT('Ctrl Pts',(-7.94384505715716,8.67361737988404E-16,
-6.63302194717649));
#4960=CARTESIAN_POINT('Ctrl Pts',(-8.1029376375198,-8.67361737988404E-16,
-6.73165714491127));
#4961=CARTESIAN_POINT('Ctrl Pts',(-8.20909022696902,0.,-6.79725491209686));
#4962=CARTESIAN_POINT('Ctrl Pts',(-8.52782105955695,0.,-6.99357032060786));
#4963=CARTESIAN_POINT('Ctrl Pts',(-8.74067236655293,0.,-7.12381006955848));
#4964=CARTESIAN_POINT('Ctrl Pts',(-9.16710559634496,-8.67361737988404E-16,
-7.38301090786864));
#4965=CARTESIAN_POINT('Ctrl Pts',(-9.38068751917746,0.,-7.51197199716448));
#4966=CARTESIAN_POINT('Ctrl Pts',(-10.0225328989281,-2.60208521396521E-15,
-7.89693082203444));
#4967=CARTESIAN_POINT('Ctrl Pts',(-10.4518959613416,0.,-8.15100412466771));
#4968=CARTESIAN_POINT('Ctrl Pts',(-11.7444133132118,0.,-8.90547424783421));
#4969=CARTESIAN_POINT('Ctrl Pts',(-12.6119956637783,-8.67361737988404E-16,
-9.39812146480502));
#4970=CARTESIAN_POINT('Ctrl Pts',(-14.3591298194595,8.67361737988404E-16,
-10.3624680108778));
#4971=CARTESIAN_POINT('Ctrl Pts',(-15.2386575500661,0.,-10.8341538011997));
#4972=CARTESIAN_POINT('Ctrl Pts',(-16.5671220278863,0.,-11.5257959301825));
#4973=CARTESIAN_POINT('Ctrl Pts',(-17.0115117764597,0.,-11.7537126716564));
#4974=CARTESIAN_POINT('Ctrl Pts',(-17.9027081412433,0.,-12.2038822495548));
#4975=CARTESIAN_POINT('Ctrl Pts',(-18.3496112197363,0.,-12.4261863775782));
#4976=CARTESIAN_POINT('Ctrl Pts',(-19.6940386192206,-8.67361737988404E-16,
-13.0846168319795));
#4977=CARTESIAN_POINT('Ctrl Pts',(-20.5954904839877,8.67361737988404E-16,
-13.5123710624704));
#4978=CARTESIAN_POINT('Ctrl Pts',(-22.4086255220037,-8.67361737988404E-16,
-14.3452323170145));
#4979=CARTESIAN_POINT('Ctrl Pts',(-23.3203377275709,0.,-14.7503544955288));
#4980=CARTESIAN_POINT('Ctrl Pts',(-25.1541238375931,0.,-15.5378229769881));
#4981=CARTESIAN_POINT('Ctrl Pts',(-26.0761731394061,0.,-15.9201593756798));
#4982=CARTESIAN_POINT('Ctrl Pts',(-28.8581207296717,0.,-17.0328234484422));
#4983=CARTESIAN_POINT('Ctrl Pts',(-30.7282718716483,0.,-17.726577311649));
#4984=CARTESIAN_POINT('Ctrl Pts',(-34.4988644814729,0.,-19.0181704069966));
#4985=CARTESIAN_POINT('Ctrl Pts',(-36.3994730456328,0.,-19.6160663145302));
#4986=CARTESIAN_POINT('Ctrl Pts',(-39.2729851137603,0.,-20.4412815926138));
#4987=CARTESIAN_POINT('Ctrl Pts',(-40.2347218365622,1.73472347597681E-15,
-20.7044462959577));
#4988=CARTESIAN_POINT('Ctrl Pts',(-41.6828409388869,0.,-21.0812937073895));
#4989=CARTESIAN_POINT('Ctrl Pts',(-42.1665408867303,8.67361737988404E-16,
-21.2039433661147));
#4990=CARTESIAN_POINT('Ctrl Pts',(-43.1357732858097,0.,-21.4432821653729));
#4991=CARTESIAN_POINT('Ctrl Pts',(-43.6214143011738,0.,-21.5599947826799));
#4992=CARTESIAN_POINT('Ctrl Pts',(-44.5936798235137,0.,-21.7872713292545));
#4993=CARTESIAN_POINT('Ctrl Pts',(-45.0804740425724,0.,-21.8978779663177));
#4994=CARTESIAN_POINT('Ctrl Pts',(-45.8115761744865,0.,-22.0592435820542));
#4995=CARTESIAN_POINT('Ctrl Pts',(-46.0554329505363,0.,-22.1122758004251));
#4996=CARTESIAN_POINT('Ctrl Pts',(-46.5434578674449,0.,-22.2168313089879));
#4997=CARTESIAN_POINT('Ctrl Pts',(-46.7876260082956,0.,-22.268354599221));
#4998=CARTESIAN_POINT('Ctrl Pts',(-47.1541111707643,0.,-22.3445106124556));
#4999=CARTESIAN_POINT('Ctrl Pts',(-47.2763117168066,0.,-22.3697077964145));
#5000=CARTESIAN_POINT('Ctrl Pts',(-47.4596707023514,0.,-22.4072216874391));
#5001=CARTESIAN_POINT('Ctrl Pts',(-47.5208000586142,0.,-22.4196793369561));
#5002=CARTESIAN_POINT('Ctrl Pts',(-47.6430781480945,0.,-22.4445007318891));
#5003=CARTESIAN_POINT('Ctrl Pts',(-47.7042270322544,0.,-22.4568637457667));
#5004=CARTESIAN_POINT('Ctrl Pts',(-47.7959644294841,0.,-22.4753400762447));
#5005=CARTESIAN_POINT('Ctrl Pts',(-47.8265467872086,0.,-22.4814832225577));
#5006=CARTESIAN_POINT('Ctrl Pts',(-47.8877124965496,0.,-22.493764698779));
#5007=CARTESIAN_POINT('Ctrl Pts',(-47.9182952814496,0.,-22.4999057748181));
#5008=CARTESIAN_POINT('Ctrl Pts',(-48.0100429184723,0.,-22.518332481796));
#5009=CARTESIAN_POINT('Ctrl Pts',(-48.0712087407834,0.,-22.5306134102228));
#5010=CARTESIAN_POINT('Ctrl Pts',(-48.193539654443,0.,-22.5551788099683));
#5011=CARTESIAN_POINT('Ctrl Pts',(-48.2547051112727,0.,-22.5674615098409));
#5012=CARTESIAN_POINT('Ctrl Pts',(-48.3770360249324,0.,-22.5920269095863));
#5013=CARTESIAN_POINT('Ctrl Pts',(-48.4382014817621,0.,-22.604309609459));
#5014=CARTESIAN_POINT('Ctrl Pts',(-48.6216978522517,0.,-22.6411577090772));
#5015=CARTESIAN_POINT('Ctrl Pts',(-48.744028765911,0.,-22.6657231088225));
#5016=CARTESIAN_POINT('Ctrl Pts',(-48.9886905932302,0.,-22.7148539083134));
#5017=CARTESIAN_POINT('Ctrl Pts',(-49.1110215068898,0.,-22.7394193080588));
#5018=CARTESIAN_POINT('Ctrl Pts',(-49.4780142478686,0.,-22.813115507295));
#5019=CARTESIAN_POINT('Ctrl Pts',(-49.7226760751877,0.,-22.8622463067859));
#5020=CARTESIAN_POINT('Ctrl Pts',(-49.9673379025068,0.,-22.9113771062766));
#5021=CARTESIAN_POINT('',(0.,0.,0.));
#5022=CARTESIAN_POINT('Origin',(21.1914505799844,-0.000524999999999484,
34.7829861880462));
#5023=CARTESIAN_POINT('',(21.1914505799844,0.,32.7829861880461));
#5024=CARTESIAN_POINT('Origin',(21.1914505799844,0.,34.7829861880462));
#5025=CARTESIAN_POINT('',(21.1914505799844,1.2,32.7829861880461));
#5026=CARTESIAN_POINT('',(21.1914505799844,-0.000524999999999484,32.7829861880462));
#5027=CARTESIAN_POINT('Origin',(21.1914505799844,1.2,34.7829861880462));
#5028=CARTESIAN_POINT('Origin',(-1.14649136662881,0.,0.));
#5029=CARTESIAN_POINT('',(-1.14649136662881,0.,-1.));
#5030=CARTESIAN_POINT('Origin',(-1.14649136662881,0.,0.));
#5031=CARTESIAN_POINT('',(-1.14649136662881,1.2,-1.));
#5032=CARTESIAN_POINT('',(-1.14649136662881,0.,-1.));
#5033=CARTESIAN_POINT('Origin',(-1.14649136662881,1.2,0.));
#5034=CARTESIAN_POINT('Ctrl Pts',(0.0163039410302629,1.2,-10.1188450599643));
#5035=CARTESIAN_POINT('Ctrl Pts',(0.0163039410302629,-0.528,-10.1188450599643));
#5036=CARTESIAN_POINT('Ctrl Pts',(-2.21904904761523,1.2,-25.218855767281));
#5037=CARTESIAN_POINT('Ctrl Pts',(-2.21904904761523,-0.528,-25.218855767281));
#5038=CARTESIAN_POINT('Ctrl Pts',(-17.3117222200821,1.2,-40.3484435255013));
#5039=CARTESIAN_POINT('Ctrl Pts',(-17.3117222200821,-0.528,-40.3484435255013));
#5040=CARTESIAN_POINT('Ctrl Pts',(-31.0970400923937,1.2,-45.9093754426411));
#5041=CARTESIAN_POINT('Ctrl Pts',(-31.0970400923937,-0.528,-45.9093754426411));
#5042=CARTESIAN_POINT('',(0.0163039410302629,0.,-10.1188450599643));
#5043=CARTESIAN_POINT('',(-29.5626263532375,-7.98607492925424E-16,-45.2534839938841));
#5044=CARTESIAN_POINT('Ctrl Pts',(0.0163039410302629,0.,-10.1188450599643));
#5045=CARTESIAN_POINT('Ctrl Pts',(-2.13636293688632,0.,-24.66030364433));
#5046=CARTESIAN_POINT('Ctrl Pts',(-16.2127531376322,0.,-39.2291916281846));
#5047=CARTESIAN_POINT('Ctrl Pts',(-29.5626263532375,0.,-45.253483993884));
#5048=CARTESIAN_POINT('',(-31.0970400928039,0.999993661824606,-45.9093754428066));
#5049=CARTESIAN_POINT('Ctrl Pts',(-29.5626263532375,-1.80411241501588E-15,
-45.2534839938841));
#5050=CARTESIAN_POINT('Ctrl Pts',(-29.8188688224744,0.163986041940123,-45.3691165190969));
#5051=CARTESIAN_POINT('Ctrl Pts',(-30.075375785987,0.329632644340004,-45.4818409421178));
#5052=CARTESIAN_POINT('Ctrl Pts',(-30.3320199519673,0.496887461248793,-45.5915431280263));
#5053=CARTESIAN_POINT('Ctrl Pts',(-30.5868401378292,0.66295359163677,-45.7004656562119));
#5054=CARTESIAN_POINT('Ctrl Pts',(-30.8418789960871,0.830662075864011,-45.806444665302));
#5055=CARTESIAN_POINT('Ctrl Pts',(-31.0970400923937,0.999993661442804,-45.9093754426411));
#5056=CARTESIAN_POINT('',(-31.0970400923937,1.2,-45.9093754426411));
#5057=CARTESIAN_POINT('',(-31.0970400923937,1.2,-45.9093754426411));
#5058=CARTESIAN_POINT('',(0.0163039410302629,1.2,-10.1188450599643));
#5059=CARTESIAN_POINT('Ctrl Pts',(0.0163039410302629,1.2,-10.1188450599643));
#5060=CARTESIAN_POINT('Ctrl Pts',(-2.21904904761523,1.2,-25.218855767281));
#5061=CARTESIAN_POINT('Ctrl Pts',(-17.3117222200821,1.2,-40.3484435255013));
#5062=CARTESIAN_POINT('Ctrl Pts',(-31.0970400923937,1.2,-45.9093754426411));
#5063=CARTESIAN_POINT('',(0.0163039410302629,1.2,-10.1188450599643));
#5064=CARTESIAN_POINT('Ctrl Pts',(-31.0970400923937,1.2,-45.9093754426411));
#5065=CARTESIAN_POINT('Ctrl Pts',(-31.0970400923937,0.911999999999981,-45.9093754426411));
#5066=CARTESIAN_POINT('Ctrl Pts',(-17.686844155281,1.2,-22.7283469888476));
#5067=CARTESIAN_POINT('Ctrl Pts',(-17.686844155281,0.911999999999981,-22.7283469888476));
#5068=CARTESIAN_POINT('Ctrl Pts',(-4.63662953841448,1.2,0.655407872751923));
#5069=CARTESIAN_POINT('Ctrl Pts',(-4.63662953841448,0.911999999999981,0.655407872751923));
#5070=CARTESIAN_POINT('',(-4.63662953868546,0.999993660672008,0.655407872945712));
#5071=CARTESIAN_POINT('Ctrl Pts',(-31.0970400923936,0.99999366103201,-45.909375442641));
#5072=CARTESIAN_POINT('Ctrl Pts',(-30.573767819807,0.999956907587257,-45.004840602375));
#5073=CARTESIAN_POINT('Ctrl Pts',(-30.0144098007429,1.00000670634066,-44.0369858115081));
#5074=CARTESIAN_POINT('Ctrl Pts',(-29.4221965441832,1.00000295949628,-43.0109978936339));
#5075=CARTESIAN_POINT('Ctrl Pts',(-28.8643920298385,0.999999430350852,-42.0446218696016));
#5076=CARTESIAN_POINT('Ctrl Pts',(-28.307044239795,0.999999999781451,-41.0779611336147));
#5077=CARTESIAN_POINT('Ctrl Pts',(-27.7501655379961,0.999999999832482,-40.1110370623424));
#5078=CARTESIAN_POINT('Ctrl Pts',(-25.6099980238801,1.0000000000286,-36.3950043261841));
#5079=CARTESIAN_POINT('Ctrl Pts',(-23.476715914865,0.999999999148073,-32.6750077927901));
#5080=CARTESIAN_POINT('Ctrl Pts',(-21.35033689032,0.999999999476567,-28.951076996802));
#5081=CARTESIAN_POINT('Ctrl Pts',(-20.0032125422252,0.999999999684679,-26.5918560921613));
#5082=CARTESIAN_POINT('Ctrl Pts',(-18.6588566071828,1.00000000011496,-24.231052287125));
#5083=CARTESIAN_POINT('Ctrl Pts',(-17.3172728840955,0.999999999975142,-21.8686720102845));
#5084=CARTESIAN_POINT('Ctrl Pts',(-15.5246981252401,0.999999999788324,-18.7121464933104));
#5085=CARTESIAN_POINT('Ctrl Pts',(-13.7370789901641,0.999999998628723,-15.5528175743293));
#5086=CARTESIAN_POINT('Ctrl Pts',(-11.9544155689351,0.999999999319974,-12.390685202677));
#5087=CARTESIAN_POINT('Ctrl Pts',(-10.6017060258834,0.999999999844504,-9.99121563114253));
#5088=CARTESIAN_POINT('Ctrl Pts',(-9.25185160494225,1.00000000000002,-7.5901347140568));
#5089=CARTESIAN_POINT('Ctrl Pts',(-7.90485658637567,1.00000000000003,-5.18745008485492));
#5090=CARTESIAN_POINT('Ctrl Pts',(-7.35921098673439,1.00000000000004,-4.21416193071989));
#5091=CARTESIAN_POINT('Ctrl Pts',(-6.814037789644,0.999999430754603,-3.24061632119799));
#5092=CARTESIAN_POINT('Ctrl Pts',(-6.26933697629459,1.00000296037334,-2.26681326697206));
#5093=CARTESIAN_POINT('Ctrl Pts',(-5.69104217874656,1.00000670767848,-1.23295169325346));
#5094=CARTESIAN_POINT('Ctrl Pts',(-5.14587265802439,0.99995690076854,-0.257068789396161));
#5095=CARTESIAN_POINT('Ctrl Pts',(-4.63662953841449,0.999993659872726,0.655407872751901));
#5096=CARTESIAN_POINT('',(-4.63662953841448,1.2,0.655407872751923));
#5097=CARTESIAN_POINT('',(-4.63662953841448,1.2,0.655407872751923));
#5098=CARTESIAN_POINT('Origin',(-3036.07761218286,1.2,1692.46950376164));
#5099=CARTESIAN_POINT('Ctrl Pts',(17.9965481466234,1.2,41.2101952278912));
#5100=CARTESIAN_POINT('Ctrl Pts',(17.9965481466234,-0.528,41.2101952278912));
#5101=CARTESIAN_POINT('Ctrl Pts',(21.1524317437801,1.2,43.1694484023668));
#5102=CARTESIAN_POINT('Ctrl Pts',(21.1524317437801,-0.528,43.1694484023668));
#5103=CARTESIAN_POINT('Ctrl Pts',(26.9936524453639,1.2,45.5981161424412));
#5104=CARTESIAN_POINT('Ctrl Pts',(26.9936524453639,-0.528,45.5981161424412));
#5105=CARTESIAN_POINT('Ctrl Pts',(33.9307266408316,1.2,41.1415677861088));
#5106=CARTESIAN_POINT('Ctrl Pts',(33.9307266408316,-0.528,41.1415677861088));
#5107=CARTESIAN_POINT('Ctrl Pts',(32.8535862824509,1.2,33.9883280103707));
#5108=CARTESIAN_POINT('Ctrl Pts',(32.8535862824509,-0.528,33.9883280103707));
#5109=CARTESIAN_POINT('Ctrl Pts',(27.9014606940056,1.2,32.3046097776791));
#5110=CARTESIAN_POINT('Ctrl Pts',(27.9014606940056,-0.528,32.3046097776791));
#5111=CARTESIAN_POINT('Ctrl Pts',(23.322809839386,1.2,30.2059351076599));
#5112=CARTESIAN_POINT('Ctrl Pts',(23.322809839386,-0.528,30.2059351076599));
#5113=CARTESIAN_POINT('Ctrl Pts',(24.7202491484524,1.2,26.5916170055359));
#5114=CARTESIAN_POINT('Ctrl Pts',(24.7202491484524,-0.528,26.5916170055359));
#5115=CARTESIAN_POINT('Ctrl Pts',(21.5911557932172,1.2,23.2911168236856));
#5116=CARTESIAN_POINT('Ctrl Pts',(21.5911557932172,-0.528,23.2911168236856));
#5117=CARTESIAN_POINT('Ctrl Pts',(18.2287371224104,1.2,27.0608466969321));
#5118=CARTESIAN_POINT('Ctrl Pts',(18.2287371224104,-0.528,27.0608466969321));
#5119=CARTESIAN_POINT('Ctrl Pts',(16.1921180788491,1.2,22.8319263998159));
#5120=CARTESIAN_POINT('Ctrl Pts',(16.1921180788491,-0.528,22.8319263998159));
#5121=CARTESIAN_POINT('Ctrl Pts',(12.9326029577631,1.2,18.8909674054421));
#5122=CARTESIAN_POINT('Ctrl Pts',(12.9326029577631,-0.528,18.8909674054421));
#5123=CARTESIAN_POINT('Ctrl Pts',(8.48253901799792,1.2,8.87740159675101));
#5124=CARTESIAN_POINT('Ctrl Pts',(8.48253901799792,-0.528,8.87740159675101));
#5125=CARTESIAN_POINT('Ctrl Pts',(1.84058088196348,1.2,2.8000810225724));
#5126=CARTESIAN_POINT('Ctrl Pts',(1.84058088196348,-0.528,2.8000810225724));
#5127=CARTESIAN_POINT('Ctrl Pts',(1.05043439536577,1.2,-3.13320072882459));
#5128=CARTESIAN_POINT('Ctrl Pts',(1.05043439536577,-0.528,-3.13320072882459));
#5129=CARTESIAN_POINT('',(17.9965481466234,0.,41.2101952278912));
#5130=CARTESIAN_POINT('',(1.05043439536577,0.,-3.13320072882459));
#5131=CARTESIAN_POINT('Ctrl Pts',(17.9965481466234,0.,41.2101952278912));
#5132=CARTESIAN_POINT('Ctrl Pts',(21.1524317437801,0.,43.1694484023668));
#5133=CARTESIAN_POINT('Ctrl Pts',(26.9936524453639,0.,45.5981161424412));
#5134=CARTESIAN_POINT('Ctrl Pts',(33.9307266408316,0.,41.1415677861088));
#5135=CARTESIAN_POINT('Ctrl Pts',(32.8535862824509,0.,33.9883280103707));
#5136=CARTESIAN_POINT('Ctrl Pts',(27.9014606940056,0.,32.3046097776791));
#5137=CARTESIAN_POINT('Ctrl Pts',(23.322809839386,0.,30.2059351076599));
#5138=CARTESIAN_POINT('Ctrl Pts',(24.7202491484524,0.,26.5916170055359));
#5139=CARTESIAN_POINT('Ctrl Pts',(21.5911557932172,0.,23.2911168236856));
#5140=CARTESIAN_POINT('Ctrl Pts',(18.2287371224104,0.,27.0608466969321));
#5141=CARTESIAN_POINT('Ctrl Pts',(16.1921180788491,0.,22.8319263998159));
#5142=CARTESIAN_POINT('Ctrl Pts',(12.9326029577631,0.,18.8909674054421));
#5143=CARTESIAN_POINT('Ctrl Pts',(8.48253901799792,0.,8.87740159675101));
#5144=CARTESIAN_POINT('Ctrl Pts',(1.84058088196348,0.,2.8000810225724));
#5145=CARTESIAN_POINT('Ctrl Pts',(1.05043439536577,0.,-3.13320072882459));
#5146=CARTESIAN_POINT('',(1.05043439536577,1.2,-3.13320072882459));
#5147=CARTESIAN_POINT('',(1.05043439536577,1.2,-3.13320072882459));
#5148=CARTESIAN_POINT('',(17.9965481466234,1.2,41.2101952278912));
#5149=CARTESIAN_POINT('Ctrl Pts',(17.9965481466234,1.2,41.2101952278912));
#5150=CARTESIAN_POINT('Ctrl Pts',(21.1524317437801,1.2,43.1694484023668));
#5151=CARTESIAN_POINT('Ctrl Pts',(26.9936524453639,1.2,45.5981161424412));
#5152=CARTESIAN_POINT('Ctrl Pts',(33.9307266408316,1.2,41.1415677861088));
#5153=CARTESIAN_POINT('Ctrl Pts',(32.8535862824509,1.2,33.9883280103707));
#5154=CARTESIAN_POINT('Ctrl Pts',(27.9014606940056,1.2,32.3046097776791));
#5155=CARTESIAN_POINT('Ctrl Pts',(23.322809839386,1.2,30.2059351076599));
#5156=CARTESIAN_POINT('Ctrl Pts',(24.7202491484524,1.2,26.5916170055359));
#5157=CARTESIAN_POINT('Ctrl Pts',(21.5911557932172,1.2,23.2911168236856));
#5158=CARTESIAN_POINT('Ctrl Pts',(18.2287371224104,1.2,27.0608466969321));
#5159=CARTESIAN_POINT('Ctrl Pts',(16.1921180788491,1.2,22.8319263998159));
#5160=CARTESIAN_POINT('Ctrl Pts',(12.9326029577631,1.2,18.8909674054421));
#5161=CARTESIAN_POINT('Ctrl Pts',(8.48253901799792,1.2,8.87740159675101));
#5162=CARTESIAN_POINT('Ctrl Pts',(1.84058088196348,1.2,2.8000810225724));
#5163=CARTESIAN_POINT('Ctrl Pts',(1.05043439536577,1.2,-3.13320072882459));
#5164=CARTESIAN_POINT('',(17.9965481466234,1.2,41.2101952278912));
#5165=CARTESIAN_POINT('Origin',(1.05043439536577,1.2,-3.13320072882459));
#5166=CARTESIAN_POINT('',(1.05043439536577,0.,-3.13320072882459));
#5167=CARTESIAN_POINT('',(1.05043439536577,1.2,-3.13320072882459));
#5168=CARTESIAN_POINT('Origin',(-11.2091312443069,1.2,-31.591264797619));
#5169=CARTESIAN_POINT('',(-4.7239511892698,1.2,0.704141119020785));
#5170=CARTESIAN_POINT('',(-4.7239511892698,1.2,0.704141119020785));
#5171=CARTESIAN_POINT('',(17.9092264957681,1.2,41.2589284741601));
#5172=CARTESIAN_POINT('',(17.9092264957681,1.2,41.2589284741601));
#5173=CARTESIAN_POINT('',(17.9092264957681,1.2,41.2589284741601));
#5174=CARTESIAN_POINT('Origin',(-11.2091312443069,0.,-31.591264797619));
#5175=CARTESIAN_POINT('',(-4.7239511892698,0.,0.704141119020785));
#5176=CARTESIAN_POINT('',(-3.7634185663843,0.,0.168078500190919));
#5177=CARTESIAN_POINT('',(-4.7239511892698,0.,0.704141119020785));
#5178=CARTESIAN_POINT('Ctrl Pts',(-3.7634185663843,0.,0.168078500190915));
#5179=CARTESIAN_POINT('Ctrl Pts',(-10.2994008356464,0.,-11.5423169605017));
#5180=CARTESIAN_POINT('Ctrl Pts',(-12.4600130210599,1.38777878078145E-15,
-15.3418604059716));
#5181=CARTESIAN_POINT('Ctrl Pts',(-20.9163234840607,1.38777878078145E-15,
-30.2298597196315));
#5182=CARTESIAN_POINT('Ctrl Pts',(-25.2491386822615,0.,-37.790624293729));
#5183=CARTESIAN_POINT('Ctrl Pts',(-29.5626263532375,0.,-45.2534839938841));
#5184=CARTESIAN_POINT('',(17.9092264957681,0.,41.2589284741601));
#5185=CARTESIAN_POINT('',(17.9092264957681,0.,41.2589284741601));
#5186=CARTESIAN_POINT('',(-4.7239511892698,0.,0.704141119020785));
#5187=CARTESIAN_POINT('Origin',(-4.7239511892698,1.2,0.704141119020785));
#5188=CARTESIAN_POINT('',(-4.6366323065132,0.99999682993773,0.655409417724869));
#5189=CARTESIAN_POINT('',(-4.7239511892698,1.2,0.704141119020785));
#5190=CARTESIAN_POINT('Origin',(17.9092264957681,0.,41.2589284741601));
#5191=CARTESIAN_POINT('',(17.9092264957681,0.,41.2589284741601));
#5192=CARTESIAN_POINT('Origin',(-3.90169114982751,0.,2.17749062010543));
#5193=CARTESIAN_POINT('Ctrl Pts',(-32.4383859892945,1.00000670767832,-48.2280289443117));
#5194=CARTESIAN_POINT('Ctrl Pts',(-32.1309955518262,1.00000670767832,-47.6966700804449));
#5195=CARTESIAN_POINT('Ctrl Pts',(-31.8236175039076,1.00000670767832,-47.1653405930931));
#5196=CARTESIAN_POINT('Ctrl Pts',(-31.2088118498719,1.00000670767832,-46.1025641123295));
#5197=CARTESIAN_POINT('Ctrl Pts',(-30.9014508032936,1.00000670767832,-45.5713166895576));
#5198=CARTESIAN_POINT('Ctrl Pts',(-29.9800401478882,1.00000670767832,-43.9775269224044));
#5199=CARTESIAN_POINT('Ctrl Pts',(-29.366284226523,1.00000670767832,-42.9145488034795));
#5200=CARTESIAN_POINT('Ctrl Pts',(-28.1399451284085,1.00000670767832,-40.7880674192455));
#5201=CARTESIAN_POINT('Ctrl Pts',(-27.5273384407701,1.00000670767832,-39.7244999614497));
#5202=CARTESIAN_POINT('Ctrl Pts',(-26.3032558235069,1.00000670767832,-37.5967201796819));
#5203=CARTESIAN_POINT('Ctrl Pts',(-25.6917792941021,1.00000670767832,-36.5325068181677));
#5204=CARTESIAN_POINT('Ctrl Pts',(-23.8590452247175,1.00000670767832,-33.3388982832929));
#5205=CARTESIAN_POINT('Ctrl Pts',(-22.6394819645239,1.00000670767832,-31.2085325126316));
#5206=CARTESIAN_POINT('Ctrl Pts',(-20.2048756335948,1.00000670767832,-26.9452159217588));
#5207=CARTESIAN_POINT('Ctrl Pts',(-18.9898323807444,1.00000670767832,-24.8122647858504));
#5208=CARTESIAN_POINT('Ctrl Pts',(-16.5642658874957,1.00000670767832,-20.5437767101294));
#5209=CARTESIAN_POINT('Ctrl Pts',(-15.3537487180158,1.00000670767832,-18.408250451539));
#5210=CARTESIAN_POINT('Ctrl Pts',(-12.9372473733207,1.00000670767832,-14.1346348557454));
#5211=CARTESIAN_POINT('Ctrl Pts',(-11.7312616183177,1.00000670767832,-11.9965427097547));
#5212=CARTESIAN_POINT('Ctrl Pts',(-9.92568646806448,1.00000670767832,-8.78748872799292));
#5213=CARTESIAN_POINT('Ctrl Pts',(-9.32439612554591,1.00000670767832,-7.71748618845371));
#5214=CARTESIAN_POINT('Ctrl Pts',(-8.12295077554065,1.00000670767832,-5.57684403913935));
#5215=CARTESIAN_POINT('Ctrl Pts',(-7.52279589125647,1.00000670767832,-4.50620464856389));
#5216=CARTESIAN_POINT('Ctrl Pts',(-6.32362169657787,1.00000670767832,-2.36428923843985));
#5217=CARTESIAN_POINT('Ctrl Pts',(-5.72456001077879,1.00000670767832,-1.29296148385365));
#5218=CARTESIAN_POINT('Ctrl Pts',(-4.82694628305467,1.00000670767832,0.314352412496741));
#5219=CARTESIAN_POINT('Ctrl Pts',(-4.52786990488178,1.00000670767832,0.850308497929449));
#5220=CARTESIAN_POINT('Ctrl Pts',(-3.92951798462665,1.00000670767832,1.92243654538334));
#5221=CARTESIAN_POINT('Ctrl Pts',(-3.63037981674452,1.00000670767832,2.45844921237444));
#5222=CARTESIAN_POINT('Ctrl Pts',(-3.33122275273957,1.00000670767832,2.99448755773365));
#5223=CARTESIAN_POINT('Ctrl Pts',(-31.5727855656386,0.,-48.7287777056367));
#5224=CARTESIAN_POINT('Ctrl Pts',(-31.2653951281703,0.,-48.1974188417698));
#5225=CARTESIAN_POINT('Ctrl Pts',(-30.9580012389628,0.,-47.666061973265));
#5226=CARTESIAN_POINT('Ctrl Pts',(-30.3432272675049,0.,-46.6033402548073));
#5227=CARTESIAN_POINT('Ctrl Pts',(-30.0358105356997,0.,-46.071996591336));
#5228=CARTESIAN_POINT('Ctrl Pts',(-29.1140850373573,0.,-44.477662286746));
#5229=CARTESIAN_POINT('Ctrl Pts',(-28.5001853221512,0.,-43.4144350187497));
#5230=CARTESIAN_POINT('Ctrl Pts',(-27.2734930129072,0.,-41.2873411637132));
#5231=CARTESIAN_POINT('Ctrl Pts',(-26.6607098789485,0.,-40.2234673714217));
#5232=CARTESIAN_POINT('Ctrl Pts',(-25.4362746895989,0.,-38.0950747259902));
#5233=CARTESIAN_POINT('Ctrl Pts',(-24.8246220342551,0.,-37.0305548350095));
#5234=CARTESIAN_POINT('Ctrl Pts',(-22.9913600686247,0.,-33.8360264209311));
#5235=CARTESIAN_POINT('Ctrl Pts',(-21.7714455193403,1.73472347597681E-15,
-31.7050470091101));
#5236=CARTESIAN_POINT('Ctrl Pts',(-19.336137898936,0.,-27.4405023679293));
#5237=CARTESIAN_POINT('Ctrl Pts',(-18.1207446456488,0.,-25.3069368227818));
#5238=CARTESIAN_POINT('Ctrl Pts',(-15.6944794449877,0.,-21.0372191686235));
#5239=CARTESIAN_POINT('Ctrl Pts',(-14.4836135702811,0.,-18.9010777439119));
#5240=CARTESIAN_POINT('Ctrl Pts',(-12.0664161170873,0.,-14.6262310707415));
#5241=CARTESIAN_POINT('Ctrl Pts',(-10.8600829583573,0.,-12.4875230126863));
#5242=CARTESIAN_POINT('Ctrl Pts',(-9.05398768358211,0.,-9.2775446120943));
#5243=CARTESIAN_POINT('Ctrl Pts',(-8.4525241299626,0.,-8.20723384156397));
#5244=CARTESIAN_POINT('Ctrl Pts',(-7.2507326856024,0.,-6.06597504816851));
#5245=CARTESIAN_POINT('Ctrl Pts',(-6.65040491809978,0.,-4.99502724456632));
#5246=CARTESIAN_POINT('Ctrl Pts',(-5.45088528547934,0.,-2.85249482746024));
#5247=CARTESIAN_POINT('Ctrl Pts',(-4.85168313295727,0.,-1.78091598210246));
#5248=CARTESIAN_POINT('Ctrl Pts',(-3.95376268794949,0.,-0.173052805131788));
#5249=CARTESIAN_POINT('Ctrl Pts',(-3.6546321212938,0.,0.363000394754204));
#5250=CARTESIAN_POINT('Ctrl Pts',(-3.05631103659737,0.,1.43507318544256));
#5251=CARTESIAN_POINT('Ctrl Pts',(-2.75715745093588,0.,1.97111348081644));
#5252=CARTESIAN_POINT('Ctrl Pts',(-2.45800038693092,0.,2.50715182617563));
#5253=CARTESIAN_POINT('',(0.,0.,0.));
#5254=CARTESIAN_POINT('Origin',(4.,0.,0.));
#5255=CARTESIAN_POINT('',(1.,-1.22464679914735E-16,-1.));
#5256=CARTESIAN_POINT('Origin',(1.,0.,0.));
#5257=CARTESIAN_POINT('',(4.,-1.22464679914735E-16,-1.));
#5258=CARTESIAN_POINT('',(4.,-1.22464679914735E-16,-1.));
#5259=CARTESIAN_POINT('Origin',(4.,0.,0.));
#5260=CARTESIAN_POINT('Origin',(1.,0.,0.));
#5261=CARTESIAN_POINT('',(0.,-1.83697019872103E-16,-1.5));
#5262=CARTESIAN_POINT('Origin',(0.,0.,0.));
#5263=CARTESIAN_POINT('',(1.,-1.83697019872103E-16,-1.5));
#5264=CARTESIAN_POINT('',(1.,-1.83697019872103E-16,-1.5));
#5265=CARTESIAN_POINT('Origin',(1.,0.,0.));
#5266=CARTESIAN_POINT('Origin',(1.,0.,0.));
#5267=CARTESIAN_POINT('Origin',(0.,0.,0.));
#5268=CARTESIAN_POINT('Origin',(4.,0.,0.));
#5269=CARTESIAN_POINT('',(-8.43445565617375,5.55433223618254,0.96471087636367));
#5270=CARTESIAN_POINT('',(-7.28796428954494,4.25433223618253,0.513328003934832));
#5271=CARTESIAN_POINT('',(-8.43445565617375,7.75433223618254,0.513328003934832));
#5272=CARTESIAN_POINT('',(0.,0.,0.));
#5273=CARTESIAN_POINT('Origin',(-1.99999999999935,42.8890026416775,0.0554857494443409));
#5274=CARTESIAN_POINT('',(-2.00000000001811,42.8890026416775,-1.69451425055565));
#5275=CARTESIAN_POINT('',(-2.00000000002259,42.8890026416775,-2.19451425055565));
#5276=CARTESIAN_POINT('Origin',(-2.00000000002035,42.8890026416775,-1.94451425055565));
#5277=CARTESIAN_POINT('Origin',(-2.00000000002035,42.8890026416775,-1.94451425055565));
#5278=CARTESIAN_POINT('',(-2.00000000001111,41.5423543458149,-1.06211810132313));
#5279=CARTESIAN_POINT('Origin',(-1.99999999999935,42.8890026416775,0.0554857494443409));
#5280=CARTESIAN_POINT('Origin',(-2.0000000000128,41.3499760178345,-1.22177579428992));
#5281=CARTESIAN_POINT('Ctrl Pts',(-2.00000000001811,42.8890026416775,-1.69451425055562));
#5282=CARTESIAN_POINT('Ctrl Pts',(-2.00000000001811,42.7138340471106,-1.69451425055564));
#5283=CARTESIAN_POINT('Ctrl Pts',(-2.00000000001811,42.5195868694293,-1.69664685121079));
#5284=CARTESIAN_POINT('Ctrl Pts',(-2.00000000001818,42.1727041659024,-1.69763022720131));
#5285=CARTESIAN_POINT('Ctrl Pts',(-2.00000000001809,42.0075453806213,-1.69643582812033));
#5286=CARTESIAN_POINT('Ctrl Pts',(-2.000000000018,41.5447432182596,-1.67506238348623));
#5287=CARTESIAN_POINT('Ctrl Pts',(-2.00000000001759,41.2824586218001,-1.63529714422004));
#5288=CARTESIAN_POINT('Ctrl Pts',(-2.00000000001559,40.8726877368524,-1.45751662005935));
#5289=CARTESIAN_POINT('Ctrl Pts',(-2.00000000001428,40.7146168625301,-1.32576584773803));
#5290=CARTESIAN_POINT('Ctrl Pts',(-2.00000000000915,40.4347106414413,-0.836444527344903));
#5291=CARTESIAN_POINT('Ctrl Pts',(-2.00000000000487,40.3213171458309,-0.475216515464907));
#5292=CARTESIAN_POINT('Ctrl Pts',(-2.,40.247426591683,0.0357782298078951));
#5293=CARTESIAN_POINT('Ctrl Pts',(-1.50000000001812,42.8890026416775,-1.69451425056007));
#5294=CARTESIAN_POINT('Ctrl Pts',(-1.50000000001811,42.7138340471107,-1.6945142505601));
#5295=CARTESIAN_POINT('Ctrl Pts',(-1.50000000001814,42.5195868694296,-1.69664685121553));
#5296=CARTESIAN_POINT('Ctrl Pts',(-1.50000000001815,42.1727041659021,-1.69763022720547));
#5297=CARTESIAN_POINT('Ctrl Pts',(-1.50000000001812,42.0075453806213,-1.69643582812505));
#5298=CARTESIAN_POINT('Ctrl Pts',(-1.50000000001802,41.5447432182596,-1.6750623834901));
#5299=CARTESIAN_POINT('Ctrl Pts',(-1.50000000001758,41.2824586218004,-1.635297144225));
#5300=CARTESIAN_POINT('Ctrl Pts',(-1.50000000001562,40.8726877368527,-1.45751662006339));
#5301=CARTESIAN_POINT('Ctrl Pts',(-1.50000000001431,40.7146168625313,-1.32576584774273));
#5302=CARTESIAN_POINT('Ctrl Pts',(-1.50000000000914,40.4347106414414,-0.836444527349893));
#5303=CARTESIAN_POINT('Ctrl Pts',(-1.50000000000502,40.321317145827,-0.475216515469928));
#5304=CARTESIAN_POINT('Ctrl Pts',(-1.5,40.2474265916837,0.0357782298028141));
#5305=CARTESIAN_POINT('Ctrl Pts',(-1.50000000002261,42.8890026416775,-2.19451425056016));
#5306=CARTESIAN_POINT('Ctrl Pts',(-1.5000000000226,42.6924352393214,-2.19451425056018));
#5307=CARTESIAN_POINT('Ctrl Pts',(-1.50000000002262,42.5242279803483,-2.196635703513));
#5308=CARTESIAN_POINT('Ctrl Pts',(-1.50000000002264,42.1708979670303,-2.19763735653693));
#5309=CARTESIAN_POINT('Ctrl Pts',(-1.50000000002256,41.9983311272475,-2.19654321697105));
#5310=CARTESIAN_POINT('Ctrl Pts',(-1.50000000002256,41.4939715199041,-2.1732505327887));
#5311=CARTESIAN_POINT('Ctrl Pts',(-1.50000000002207,41.1721096008011,-2.1324514159462));
#5312=CARTESIAN_POINT('Ctrl Pts',(-1.50000000001927,40.5850276451855,-1.87774381002253));
#5313=CARTESIAN_POINT('Ctrl Pts',(-1.50000000001706,40.3267157332556,-1.65463617720806));
#5314=CARTESIAN_POINT('Ctrl Pts',(-1.50000000001012,39.9545934323558,-1.00410633608771));
#5315=CARTESIAN_POINT('Ctrl Pts',(-1.50000000000546,39.831903366932,-0.584389540167537));
#5316=CARTESIAN_POINT('Ctrl Pts',(-1.50000000000002,39.752573408318,-0.0357782298130924));
#5317=CARTESIAN_POINT('Ctrl Pts',(-2.00000000002259,42.8890026416775,-2.19451425055564));
#5318=CARTESIAN_POINT('Ctrl Pts',(-2.0000000000226,42.6924352393214,-2.19451425055565));
#5319=CARTESIAN_POINT('Ctrl Pts',(-2.00000000002263,42.5242279803487,-2.19663570350848));
#5320=CARTESIAN_POINT('Ctrl Pts',(-2.00000000002263,42.17089796703,-2.19763735653241));
#5321=CARTESIAN_POINT('Ctrl Pts',(-2.00000000002255,41.9983311272475,-2.19654321696658));
#5322=CARTESIAN_POINT('Ctrl Pts',(-2.00000000002255,41.4939715199041,-2.17325053278423));
#5323=CARTESIAN_POINT('Ctrl Pts',(-2.00000000002206,41.1721096008009,-2.13245141594075));
#5324=CARTESIAN_POINT('Ctrl Pts',(-2.00000000001923,40.5850276451852,-1.87774381001891));
#5325=CARTESIAN_POINT('Ctrl Pts',(-2.00000000001706,40.3267157332544,-1.65463617720347));
#5326=CARTESIAN_POINT('Ctrl Pts',(-2.00000000001007,39.9545934323557,-1.0041063360826));
#5327=CARTESIAN_POINT('Ctrl Pts',(-2.00000000000546,39.8319033669359,-0.58438954016253));
#5328=CARTESIAN_POINT('Ctrl Pts',(-2.,39.7525734083173,-0.03577822980802));
#5329=CARTESIAN_POINT('Ctrl Pts',(-2.50000000002261,42.8890026416775,-2.19451425055115));
#5330=CARTESIAN_POINT('Ctrl Pts',(-2.5000000000226,42.6924352393213,-2.19451425055115));
#5331=CARTESIAN_POINT('Ctrl Pts',(-2.50000000002264,42.524227980349,-2.19663570350397));
#5332=CARTESIAN_POINT('Ctrl Pts',(-2.50000000002262,42.1708979670296,-2.19763735652791));
#5333=CARTESIAN_POINT('Ctrl Pts',(-2.50000000002255,41.9983311272475,-2.19654321696204));
#5334=CARTESIAN_POINT('Ctrl Pts',(-2.50000000002259,41.493971519904,-2.17325053277969));
#5335=CARTESIAN_POINT('Ctrl Pts',(-2.5000000000221,41.1721096008005,-2.13245141593522));
#5336=CARTESIAN_POINT('Ctrl Pts',(-2.50000000001924,40.5850276451849,-1.87774381001523));
#5337=CARTESIAN_POINT('Ctrl Pts',(-2.50000000001709,40.3267157332532,-1.65463617719887));
#5338=CARTESIAN_POINT('Ctrl Pts',(-2.50000000001009,39.9545934323556,-1.00410633607742));
#5339=CARTESIAN_POINT('Ctrl Pts',(-2.50000000000545,39.8319033669398,-0.584389540157467));
#5340=CARTESIAN_POINT('Ctrl Pts',(-2.50000000000002,39.7525734083165,-0.0357782298028245));
#5341=CARTESIAN_POINT('Ctrl Pts',(-2.50000000001813,42.8890026416775,-1.69451425055113));
#5342=CARTESIAN_POINT('Ctrl Pts',(-2.50000000001811,42.7138340471106,-1.69451425055112));
#5343=CARTESIAN_POINT('Ctrl Pts',(-2.50000000001808,42.519586869429,-1.69664685120596));
#5344=CARTESIAN_POINT('Ctrl Pts',(-2.50000000001821,42.1727041659027,-1.6976302271971));
#5345=CARTESIAN_POINT('Ctrl Pts',(-2.50000000001814,42.0075453806212,-1.69643582811551));
#5346=CARTESIAN_POINT('Ctrl Pts',(-2.50000000001799,41.5447432182596,-1.67506238348225));
#5347=CARTESIAN_POINT('Ctrl Pts',(-2.50000000001761,41.2824586217998,-1.63529714421497));
#5348=CARTESIAN_POINT('Ctrl Pts',(-2.5000000000156,40.872687736852,-1.45751662005523));
#5349=CARTESIAN_POINT('Ctrl Pts',(-2.50000000001424,40.7146168625289,-1.32576584773326));
#5350=CARTESIAN_POINT('Ctrl Pts',(-2.50000000000921,40.4347106414412,-0.836444527339844));
#5351=CARTESIAN_POINT('Ctrl Pts',(-2.50000000000473,40.3213171458348,-0.475216515459863));
#5352=CARTESIAN_POINT('Ctrl Pts',(-2.5,40.2474265916822,0.0357782298130767));
#5353=CARTESIAN_POINT('Ctrl Pts',(-2.00000000001811,42.8890026416775,-1.69451425055562));
#5354=CARTESIAN_POINT('Ctrl Pts',(-2.00000000001811,42.7138340471106,-1.69451425055564));
#5355=CARTESIAN_POINT('Ctrl Pts',(-2.00000000001811,42.5195868694293,-1.69664685121079));
#5356=CARTESIAN_POINT('Ctrl Pts',(-2.00000000001818,42.1727041659024,-1.69763022720131));
#5357=CARTESIAN_POINT('Ctrl Pts',(-2.00000000001809,42.0075453806213,-1.69643582812033));
#5358=CARTESIAN_POINT('Ctrl Pts',(-2.000000000018,41.5447432182596,-1.67506238348623));
#5359=CARTESIAN_POINT('Ctrl Pts',(-2.00000000001759,41.2824586218001,-1.63529714422004));
#5360=CARTESIAN_POINT('Ctrl Pts',(-2.00000000001559,40.8726877368524,-1.45751662005935));
#5361=CARTESIAN_POINT('Ctrl Pts',(-2.00000000001428,40.7146168625301,-1.32576584773803));
#5362=CARTESIAN_POINT('Ctrl Pts',(-2.00000000000915,40.4347106414413,-0.836444527344903));
#5363=CARTESIAN_POINT('Ctrl Pts',(-2.00000000000487,40.3213171458309,-0.475216515464907));
#5364=CARTESIAN_POINT('Ctrl Pts',(-2.,40.247426591683,0.0357782298078951));
#5365=CARTESIAN_POINT('',(-1.99999999998774,39.7613743993598,-0.0949461097254665));
#5366=CARTESIAN_POINT('Ctrl Pts',(-2.00000000002259,42.8890026416775,-2.19451425055565));
#5367=CARTESIAN_POINT('Ctrl Pts',(-2.0000000000226,42.6924352393214,-2.19451425055565));
#5368=CARTESIAN_POINT('Ctrl Pts',(-2.00000000002263,42.5242279803487,-2.19663570350848));
#5369=CARTESIAN_POINT('Ctrl Pts',(-2.00000000002263,42.17089796703,-2.19763735653241));
#5370=CARTESIAN_POINT('Ctrl Pts',(-2.00000000002255,41.9983311272475,-2.19654321696658));
#5371=CARTESIAN_POINT('Ctrl Pts',(-2.00000000002255,41.4939715199041,-2.17325053278423));
#5372=CARTESIAN_POINT('Ctrl Pts',(-2.00000000002206,41.1721096008009,-2.13245141594075));
#5373=CARTESIAN_POINT('Ctrl Pts',(-2.00000000001923,40.5850276451852,-1.87774381001891));
#5374=CARTESIAN_POINT('Ctrl Pts',(-2.00000000001706,40.3267157332544,-1.65463617720347));
#5375=CARTESIAN_POINT('Ctrl Pts',(-2.0000000000102,39.9613396308944,-1.01589977993944));
#5376=CARTESIAN_POINT('Ctrl Pts',(-2.00000000000579,39.8408836611054,-0.61470152310314));
#5377=CARTESIAN_POINT('Ctrl Pts',(-1.99999999998774,39.7613743993598,-0.0949461097254665));
#5378=CARTESIAN_POINT('',(-2.24999999999999,40.0000000000105,4.08006961549745E-12));
#5379=CARTESIAN_POINT('Origin',(-1.99953720054553,40.0004045586706,0.000160968780395163));
#5380=CARTESIAN_POINT('',(-2.00000000002568,40.247426591683,0.0357782298078905));
#5381=CARTESIAN_POINT('Origin',(-1.99999999999999,40.0000000000001,-6.24500451351651E-14));
#5382=CARTESIAN_POINT('Ctrl Pts',(-2.00000000001811,42.8890026416775,-1.69451425055565));
#5383=CARTESIAN_POINT('Ctrl Pts',(-2.00000000001811,42.7138340471106,-1.69451425055564));
#5384=CARTESIAN_POINT('Ctrl Pts',(-2.00000000001811,42.5195868694293,-1.69664685121079));
#5385=CARTESIAN_POINT('Ctrl Pts',(-2.00000000001818,42.1727041659024,-1.69763022720131));
#5386=CARTESIAN_POINT('Ctrl Pts',(-2.00000000001809,42.0075453806213,-1.69643582812033));
#5387=CARTESIAN_POINT('Ctrl Pts',(-2.000000000018,41.5447432182596,-1.67506238348623));
#5388=CARTESIAN_POINT('Ctrl Pts',(-2.00000000001759,41.2824586218001,-1.63529714422004));
#5389=CARTESIAN_POINT('Ctrl Pts',(-2.00000000001559,40.8726877368524,-1.45751662005935));
#5390=CARTESIAN_POINT('Ctrl Pts',(-2.00000000001428,40.7146168625301,-1.32576584773803));
#5391=CARTESIAN_POINT('Ctrl Pts',(-2.00000000000915,40.4347106414413,-0.836444527344903));
#5392=CARTESIAN_POINT('Ctrl Pts',(-2.00000000000487,40.3213171458309,-0.475216515464907));
#5393=CARTESIAN_POINT('Ctrl Pts',(-2.00000000002568,40.247426591683,0.0357782298078905));
#5394=CARTESIAN_POINT('Ctrl Pts',(-2.,-0.264726219523816,0.141138331776411));
#5395=CARTESIAN_POINT('Ctrl Pts',(-1.93317897182823,-0.140204737359338,
0.374697162628536));
#5396=CARTESIAN_POINT('Ctrl Pts',(-1.89576248628645,-0.0714193310070166,
0.563392832565318));
#5397=CARTESIAN_POINT('Ctrl Pts',(-1.85828016234107,-0.0141476745355931,
0.845995304749381));
#5398=CARTESIAN_POINT('Ctrl Pts',(-1.85721582540971,-0.0237125088868792,
0.935184056400945));
#5399=CARTESIAN_POINT('Ctrl Pts',(-1.86061638209651,-0.0666740172427863,
1.06187361715673));
#5400=CARTESIAN_POINT('Ctrl Pts',(-1.86640738686477,-0.101672715288381,
1.11012925637074));
#5401=CARTESIAN_POINT('Ctrl Pts',(-1.88833554246329,-0.235746153313808,
1.21545234876845));
#5402=CARTESIAN_POINT('Ctrl Pts',(-1.9033753276643,-0.335251316849042,1.26604967753693));
#5403=CARTESIAN_POINT('Ctrl Pts',(-1.9189176957612,-0.518726439558199,1.34035163842065));
#5404=CARTESIAN_POINT('Ctrl Pts',(-1.92137116451861,-0.585485291115871,
1.36832017615168));
#5405=CARTESIAN_POINT('Ctrl Pts',(-1.93896943688162,-0.724455435049461,
1.40322870297494));
#5406=CARTESIAN_POINT('Ctrl Pts',(-1.95325668725115,-0.796545227124419,
1.40888781048668));
#5407=CARTESIAN_POINT('Ctrl Pts',(-1.99209925627655,-1.01599260874888,1.41219882843878));
#5408=CARTESIAN_POINT('Ctrl Pts',(-2.00898122237353,-1.16761549888469,1.40420126611032));
#5409=CARTESIAN_POINT('Ctrl Pts',(-2.01271588366055,-1.60175062040053,1.36576567629003));
#5410=CARTESIAN_POINT('Ctrl Pts',(-1.95046360827934,-1.85129221142242,1.32547580954877));
#5411=CARTESIAN_POINT('Ctrl Pts',(-1.69792570410908,-2.14007513561928,1.27973035876422));
#5412=CARTESIAN_POINT('Ctrl Pts',(-1.50788517190343,-2.24578075342313,1.26508664601861));
#5413=CARTESIAN_POINT('Ctrl Pts',(-1.03351721040672,-2.37409803162741,1.24662061906772));
#5414=CARTESIAN_POINT('Ctrl Pts',(-0.753928362614793,-2.39679255199907,
1.24243205928811));
#5415=CARTESIAN_POINT('Ctrl Pts',(-0.218845999430284,-2.35785399723118,
1.24055602083421));
#5416=CARTESIAN_POINT('Ctrl Pts',(0.0368662467341799,-2.29519092886669,
1.24322556456469));
#5417=CARTESIAN_POINT('Ctrl Pts',(0.411239882065782,-2.11406967659605,1.2495991139221));
#5418=CARTESIAN_POINT('Ctrl Pts',(0.518384719875618,-2.00298884738698,1.25072899682664));
#5419=CARTESIAN_POINT('Ctrl Pts',(0.571801954928687,-1.83523605217566,1.25334679757698));
#5420=CARTESIAN_POINT('Ctrl Pts',(0.569023344394799,-1.74044478899434,1.25599881503435));
#5421=CARTESIAN_POINT('Ctrl Pts',(0.494126240428662,-1.50788563057796,1.25886663470126));
#5422=CARTESIAN_POINT('Ctrl Pts',(0.421606239831573,-1.37485017740085,1.26041038383949));
#5423=CARTESIAN_POINT('Ctrl Pts',(0.127609128452456,-0.989034614321357,
1.26907008807672));
#5424=CARTESIAN_POINT('Ctrl Pts',(-0.170570542490676,-0.751894328558357,
1.28023791867232));
#5425=CARTESIAN_POINT('Ctrl Pts',(-0.569600762546571,-0.586703644418381,
1.30640573381989));
#5426=CARTESIAN_POINT('Ctrl Pts',(-0.692371618949951,-0.563856396440986,
1.31685387723007));
#5427=CARTESIAN_POINT('Ctrl Pts',(-0.882581236630141,-0.577499841895708,
1.33968897633028));
#5428=CARTESIAN_POINT('Ctrl Pts',(-0.949730803773584,-0.6053755874494,1.35084566027416));
#5429=CARTESIAN_POINT('Ctrl Pts',(-1.08267031338154,-0.742643707380371,
1.38530535019886));
#5430=CARTESIAN_POINT('Ctrl Pts',(-1.14980571385887,-0.863823663666268,
1.41045379245241));
#5431=CARTESIAN_POINT('Ctrl Pts',(-1.22863752459304,-1.27359538565792,1.48274964800499));
#5432=CARTESIAN_POINT('Ctrl Pts',(-1.23841278692706,-1.55826711159036,1.52914339518866));
#5433=CARTESIAN_POINT('Ctrl Pts',(-1.19858468901873,-1.92998306793573,1.58589472341859));
#5434=CARTESIAN_POINT('Ctrl Pts',(-1.41479497306135,-0.327024714779108,
0.0242881116882445));
#5435=CARTESIAN_POINT('Ctrl Pts',(-1.34348834763361,-0.181249481177505,
0.268980137453439));
#5436=CARTESIAN_POINT('Ctrl Pts',(-1.3008279414714,-0.0880635038225108,
0.476394018094572));
#5437=CARTESIAN_POINT('Ctrl Pts',(-1.25754057161045,0.0123013660558204,
0.831666797361881));
#5438=CARTESIAN_POINT('Ctrl Pts',(-1.25687388480527,0.0194522591100595,
0.979479411006855));
#5439=CARTESIAN_POINT('Ctrl Pts',(-1.2830830371466,-0.0336379080354797,
1.23391882276437));
#5440=CARTESIAN_POINT('Ctrl Pts',(-1.30959041125068,-0.0938600720654208,
1.34021747917579));
#5441=CARTESIAN_POINT('Ctrl Pts',(-1.38041341547889,-0.261824969553754,
1.53853407301497));
#5442=CARTESIAN_POINT('Ctrl Pts',(-1.42362766577653,-0.369411940643664,
1.63197959161429));
#5443=CARTESIAN_POINT('Ctrl Pts',(-1.51482462448403,-0.553055900414141,
1.7840154902546));
#5444=CARTESIAN_POINT('Ctrl Pts',(-1.55452145207106,-0.616871235334267,
1.84288502733572));
#5445=CARTESIAN_POINT('Ctrl Pts',(-1.61769237293684,-0.76088554847919,1.90941994885935));
#5446=CARTESIAN_POINT('Ctrl Pts',(-1.63741652204799,-0.839819060706829,
1.91721278463516));
#5447=CARTESIAN_POINT('Ctrl Pts',(-1.67857813189676,-1.07311708366726,1.92065626175757));
#5448=CARTESIAN_POINT('Ctrl Pts',(-1.69450638574114,-1.22468485755413,1.91207917479615));
#5449=CARTESIAN_POINT('Ctrl Pts',(-1.69776273723848,-1.63025676912522,1.87601769283407));
#5450=CARTESIAN_POINT('Ctrl Pts',(-1.63558587031057,-1.8094473554909,1.8484014728917));
#5451=CARTESIAN_POINT('Ctrl Pts',(-1.51744170723058,-1.93391724344097,1.82161070104937));
#5452=CARTESIAN_POINT('Ctrl Pts',(-1.38720614355509,-2.01215777720118,1.80651658245784));
#5453=CARTESIAN_POINT('Ctrl Pts',(-0.999318445532683,-2.1000372109959,1.78142022672165));
#5454=CARTESIAN_POINT('Ctrl Pts',(-0.75320228279494,-2.109345485096,1.77049841986191));
#5455=CARTESIAN_POINT('Ctrl Pts',(-0.291144343481196,-2.05182844476988,
1.75300283223748));
#5456=CARTESIAN_POINT('Ctrl Pts',(-0.0746276920240247,-1.98390441220646,
1.74716065612451));
#5457=CARTESIAN_POINT('Ctrl Pts',(0.192072445804306,-1.83915272276575,1.73915712563726));
#5458=CARTESIAN_POINT('Ctrl Pts',(0.210347585325089,-1.77773490581458,1.73080489996179));
#5459=CARTESIAN_POINT('Ctrl Pts',(0.198976982175155,-1.81462152515841,1.73113541660097));
#5460=CARTESIAN_POINT('Ctrl Pts',(0.213011996067426,-1.79205629656322,1.73877515384333));
#5461=CARTESIAN_POINT('Ctrl Pts',(0.177186567758258,-1.65070903664641,1.7504269870299));
#5462=CARTESIAN_POINT('Ctrl Pts',(0.129908624188708,-1.54404411523484,1.75773877200305));
#5463=CARTESIAN_POINT('Ctrl Pts',(-0.0876107518951426,-1.21505608778235,
1.78559033317587));
#5464=CARTESIAN_POINT('Ctrl Pts',(-0.337497876869364,-0.989695956702306,
1.81129298511067));
#5465=CARTESIAN_POINT('Ctrl Pts',(-0.619417429815987,-0.851281642971048,
1.84410939565886));
#5466=CARTESIAN_POINT('Ctrl Pts',(-0.691821618472955,-0.839216119419207,
1.85456575460658));
#5467=CARTESIAN_POINT('Ctrl Pts',(-0.742506322151624,-0.836948971076064,
1.86696729841403));
#5468=CARTESIAN_POINT('Ctrl Pts',(-0.720038690828119,-0.826234748910869,
1.86596691745099));
#5469=CARTESIAN_POINT('Ctrl Pts',(-0.741001371120147,-0.843622783703197,
1.87515508429125));
#5470=CARTESIAN_POINT('Ctrl Pts',(-0.787635764756597,-0.899635885793011,
1.88970955146323));
#5471=CARTESIAN_POINT('Ctrl Pts',(-0.852118294742336,-1.21903207139812,
1.94900258458685));
#5472=CARTESIAN_POINT('Ctrl Pts',(-0.865431353370241,-1.47313529513962,
1.99195746223939));
#5473=CARTESIAN_POINT('Ctrl Pts',(-0.829509728173782,-1.82164035961998,
2.04637874141716));
#5474=CARTESIAN_POINT('Ctrl Pts',(-1.41479497306136,0.202427724268475,-0.257988551864688));
#5475=CARTESIAN_POINT('Ctrl Pts',(-1.34782648899619,0.367997360937599,0.023830846800561));
#5476=CARTESIAN_POINT('Ctrl Pts',(-1.30808707499932,0.484781686762276,0.280931411872746));
#5477=CARTESIAN_POINT('Ctrl Pts',(-1.27980253042162,0.615948260124595,0.792619532033457));
#5478=CARTESIAN_POINT('Ctrl Pts',(-1.29321476237305,0.626404567290167,1.05659684088554));
#5479=CARTESIAN_POINT('Ctrl Pts',(-1.38946357811,0.488938846353634,1.53600410055517));
#5480=CARTESIAN_POINT('Ctrl Pts',(-1.46927966447622,0.34423952699714,1.72959611556546));
#5481=CARTESIAN_POINT('Ctrl Pts',(-1.64804633832672,0.0351654638783543,
1.99593663738672));
#5482=CARTESIAN_POINT('Ctrl Pts',(-1.74809047347069,-0.128192913728382,
2.08305283586927));
#5483=CARTESIAN_POINT('Ctrl Pts',(-1.93188952347472,-0.373532157725284,
2.17842710957436));
#5484=CARTESIAN_POINT('Ctrl Pts',(-2.00679552031709,-0.454457191434216,
2.20361434518665));
#5485=CARTESIAN_POINT('Ctrl Pts',(-2.10891108326887,-0.632484078259461,
2.2307813240385));
#5486=CARTESIAN_POINT('Ctrl Pts',(-2.13408587854556,-0.728563548890991,
2.23545023463704));
#5487=CARTESIAN_POINT('Ctrl Pts',(-2.18470343784499,-1.01580120595979,2.23985105426332));
#5488=CARTESIAN_POINT('Ctrl Pts',(-2.20504953495422,-1.20449005728727,2.22965055680831));
#5489=CARTESIAN_POINT('Ctrl Pts',(-2.20926209776938,-1.74080899784122,2.18228791128134));
#5490=CARTESIAN_POINT('Ctrl Pts',(-2.13571406139752,-2.05748394873335,2.12938063388729));
#5491=CARTESIAN_POINT('Ctrl Pts',(-1.80914039490605,-2.4116424454986,2.07707686166329));
#5492=CARTESIAN_POINT('Ctrl Pts',(-1.58558544675306,-2.52101501223511,2.06437413078064));
#5493=CARTESIAN_POINT('Ctrl Pts',(-1.06274917012361,-2.63535508293751,2.05380211046861));
#5494=CARTESIAN_POINT('Ctrl Pts',(-0.765526424774163,-2.63982623851908,
2.05574575179177));
#5495=CARTESIAN_POINT('Ctrl Pts',(-0.201198256641021,-2.55922793898205,
2.06506565863797));
#5496=CARTESIAN_POINT('Ctrl Pts',(0.0660448366282887,-2.47511972447648,
2.07245950804548));
#5497=CARTESIAN_POINT('Ctrl Pts',(0.475148760175511,-2.24745677674094,2.08564829134537));
#5498=CARTESIAN_POINT('Ctrl Pts',(0.608134614732898,-2.10455710556735,2.09040062351607));
#5499=CARTESIAN_POINT('Ctrl Pts',(0.692807377742016,-1.84294516771091,2.09414100985965));
#5500=CARTESIAN_POINT('Ctrl Pts',(0.695288539321058,-1.71667259554446,2.09510414856687));
#5501=CARTESIAN_POINT('Ctrl Pts',(0.624899286559479,-1.43522068083482,2.09446462416269));
#5502=CARTESIAN_POINT('Ctrl Pts',(0.555414215357652,-1.2826933626758,2.0935057350151));
#5503=CARTESIAN_POINT('Ctrl Pts',(0.273957080557801,-0.835699802377016,
2.09178023085904));
#5504=CARTESIAN_POINT('Ctrl Pts',(-0.0144466890476935,-0.553079604701429,
2.09136454656141));
#5505=CARTESIAN_POINT('Ctrl Pts',(-0.45094860176887,-0.336574440271572,
2.10878602648762));
#5506=CARTESIAN_POINT('Ctrl Pts',(-0.595413630263608,-0.298852315146673,
2.11776209928019));
#5507=CARTESIAN_POINT('Ctrl Pts',(-0.85098489192329,-0.305627887932605,
2.14353553496541));
#5508=CARTESIAN_POINT('Ctrl Pts',(-0.96192160586922,-0.346842648185032,
2.15984784684465));
#5509=CARTESIAN_POINT('Ctrl Pts',(-1.15250413694999,-0.533505951798014,
2.20558401172234));
#5510=CARTESIAN_POINT('Ctrl Pts',(-1.23266332711506,-0.683289971881234,
2.23568288668276));
#5511=CARTESIAN_POINT('Ctrl Pts',(-1.32515666438693,-1.13327359192835,2.31428720538256));
#5512=CARTESIAN_POINT('Ctrl Pts',(-1.33679811649895,-1.43203332580916,2.36251628262105));
#5513=CARTESIAN_POINT('Ctrl Pts',(-1.29844891076763,-1.81475034924797,2.42060937990806));
#5514=CARTESIAN_POINT('Ctrl Pts',(-1.99999999999999,0.264726219523767,-0.14113833177655));
#5515=CARTESIAN_POINT('Ctrl Pts',(-1.93751711319081,0.409042104755758,0.129547871975604));
#5516=CARTESIAN_POINT('Ctrl Pts',(-1.9030216198144,0.501425859577798,0.367930226343516));
#5517=CARTESIAN_POINT('Ctrl Pts',(-1.88054212115223,0.589499219533149,0.806948039420934));
#5518=CARTESIAN_POINT('Ctrl Pts',(-1.89355670297749,0.583239799293228,1.01230148627963));
#5519=CARTESIAN_POINT('Ctrl Pts',(-1.96699692305992,0.455902737146338,1.36395889494755));
#5520=CARTESIAN_POINT('Ctrl Pts',(-2.02609664009031,0.336426883774145,1.4995078927604));
#5521=CARTESIAN_POINT('Ctrl Pts',(-2.15596846531113,0.0612442801182847,
1.67285491314019));
#5522=CARTESIAN_POINT('Ctrl Pts',(-2.22783813535845,-0.0940322899337931,
1.71712292179187));
#5523=CARTESIAN_POINT('Ctrl Pts',(-2.33598259475191,-0.33920269686933,1.73476325774032));
#5524=CARTESIAN_POINT('Ctrl Pts',(-2.37364523276466,-0.423071247215849,
1.72904949400271));
#5525=CARTESIAN_POINT('Ctrl Pts',(-2.43018814721365,-0.596053964829743,
1.72459007815411));
#5526=CARTESIAN_POINT('Ctrl Pts',(-2.44992604374876,-0.685289715308575,
1.72712526048845));
#5527=CARTESIAN_POINT('Ctrl Pts',(-2.49822456222477,-0.958676731041413,
1.73139362094456));
#5528=CARTESIAN_POINT('Ctrl Pts',(-2.51952437158661,-1.14742069861778,1.72177264812241));
#5529=CARTESIAN_POINT('Ctrl Pts',(-2.52421524419146,-1.71230284911647,1.67203589473725));
#5530=CARTESIAN_POINT('Ctrl Pts',(-2.45059179936626,-2.09932880466486,1.60645497054434));
#5531=CARTESIAN_POINT('Ctrl Pts',(-1.98962439178456,-2.61780033767695,1.53519651937827));
#5532=CARTESIAN_POINT('Ctrl Pts',(-1.70626447510137,-2.75463798845714,1.52294419434135));
#5533=CARTESIAN_POINT('Ctrl Pts',(-1.09694793499771,-2.90941590356896,1.5190025028147));
#5534=CARTESIAN_POINT('Ctrl Pts',(-0.766252504594009,-2.92727330542218,
1.52767939121794));
#5535=CARTESIAN_POINT('Ctrl Pts',(-0.128899912590116,-2.86525349144335,
1.55261884723468));
#5536=CARTESIAN_POINT('Ctrl Pts',(0.177538775386479,-2.78640624113666,1.56852441648561));
#5537=CARTESIAN_POINT('Ctrl Pts',(0.694316196436971,-2.52237373057128,1.59609027963019));
#5538=CARTESIAN_POINT('Ctrl Pts',(0.916171749283459,-2.32981104713974,1.610324720381));
#5539=CARTESIAN_POINT('Ctrl Pts',(1.06563235049552,-1.86355969472816,1.61635239083565));
#5540=CARTESIAN_POINT('Ctrl Pts',(1.05129988764842,-1.66506108797555,1.61232780975798));
#5541=CARTESIAN_POINT('Ctrl Pts',(0.941838959229918,-1.29239727476634,1.60290427183405));
#5542=CARTESIAN_POINT('Ctrl Pts',(0.847111831000521,-1.11349942484178,1.59617734685152));
#5543=CARTESIAN_POINT('Ctrl Pts',(0.48917696090542,-0.609678328916015,1.57525998575984));
#5544=CARTESIAN_POINT('Ctrl Pts',(0.152480645331013,-0.315277976557456,
1.560309480123));
#5545=CARTESIAN_POINT('Ctrl Pts',(-0.401131934499451,-0.0719964417188537,
1.57108236464872));
#5546=CARTESIAN_POINT('Ctrl Pts',(-0.595963630740598,-0.0234925921684045,
1.58005022190368));
#5547=CARTESIAN_POINT('Ctrl Pts',(-0.99105980640179,-0.0461787587522702,
1.61625721288154));
#5548=CARTESIAN_POINT('Ctrl Pts',(-1.19161371881466,-0.12598348672354,1.64472658966789));
#5549=CARTESIAN_POINT('Ctrl Pts',(-1.49417307921139,-0.432526875475132,
1.71573427762991));
#5550=CARTESIAN_POINT('Ctrl Pts',(-1.5948332762173,-0.647477749754412,1.75642712767188));
#5551=CARTESIAN_POINT('Ctrl Pts',(-1.70167589423767,-1.18783690618816,1.84803426880073));
#5552=CARTESIAN_POINT('Ctrl Pts',(-1.70977955005583,-1.51716514225989,1.89970221556995));
#5553=CARTESIAN_POINT('Ctrl Pts',(-1.66752387161256,-1.92309305756368,1.96012536190953));
#5554=CARTESIAN_POINT('Ctrl Pts',(-2.58520502693868,0.327024714779061,-0.0242881116882809));
#5555=CARTESIAN_POINT('Ctrl Pts',(-2.52720773738545,0.450086848573887,0.235264897150667));
#5556=CARTESIAN_POINT('Ctrl Pts',(-2.49795616462949,0.518070032393306,0.45492904081419));
#5557=CARTESIAN_POINT('Ctrl Pts',(-2.48128171188284,0.563050178941749,0.821276546808376));
#5558=CARTESIAN_POINT('Ctrl Pts',(-2.49389864358196,0.540075031296315,0.968006131673827));
#5559=CARTESIAN_POINT('Ctrl Pts',(-2.54453026800985,0.422866627938986,1.19191368933997));
#5560=CARTESIAN_POINT('Ctrl Pts',(-2.58291361570442,0.32861424055116,1.26941966995528));
#5561=CARTESIAN_POINT('Ctrl Pts',(-2.66389059229556,0.0873230963582133,
1.34977318889387));
#5562=CARTESIAN_POINT('Ctrl Pts',(-2.70758579724625,-0.0598716661391885,
1.35119300771448));
#5563=CARTESIAN_POINT('Ctrl Pts',(-2.74007566602911,-0.304873236013411,
1.29109940590619));
#5564=CARTESIAN_POINT('Ctrl Pts',(-2.74049494521224,-0.391685302997432,
1.25448464281861));
#5565=CARTESIAN_POINT('Ctrl Pts',(-2.75146521115844,-0.559623851400008,
1.21839883226965));
#5566=CARTESIAN_POINT('Ctrl Pts',(-2.76576620895198,-0.642015881726228,
1.21880028633987));
#5567=CARTESIAN_POINT('Ctrl Pts',(-2.81174568660457,-0.901552256123071,
1.22293618762564));
#5568=CARTESIAN_POINT('Ctrl Pts',(-2.83399920821904,-1.09035133994834,1.21389473943648));
#5569=CARTESIAN_POINT('Ctrl Pts',(-2.83916839061358,-1.68379670039174,1.16178387819315));
#5570=CARTESIAN_POINT('Ctrl Pts',(-2.76546953733502,-2.14117366059643,1.08352930720148));
#5571=CARTESIAN_POINT('Ctrl Pts',(-2.17010838866312,-2.82395822985523,0.99331617709322));
#5572=CARTESIAN_POINT('Ctrl Pts',(-1.8269435034497,-2.98826096467916,0.981514257902072));
#5573=CARTESIAN_POINT('Ctrl Pts',(-1.13114669987181,-3.18347672420042,0.984202895160761));
#5574=CARTESIAN_POINT('Ctrl Pts',(-0.766978584413879,-3.21472037232524,
0.99961303064418));
#5575=CARTESIAN_POINT('Ctrl Pts',(-0.0566015685392616,-3.1712790439046,
1.04017203583152));
#5576=CARTESIAN_POINT('Ctrl Pts',(0.289032714144647,-3.09769275779683,1.0645893249258));
#5577=CARTESIAN_POINT('Ctrl Pts',(0.913483632698393,-2.79729068440162,1.10653226791493));
#5578=CARTESIAN_POINT('Ctrl Pts',(1.22420888383399,-2.55506498871208,1.13024881724595));
#5579=CARTESIAN_POINT('Ctrl Pts',(1.43845732324901,-1.88417422174541,1.13856377181168));
#5580=CARTESIAN_POINT('Ctrl Pts',(1.40731123597572,-1.61344958040663,1.12955147094911));
#5581=CARTESIAN_POINT('Ctrl Pts',(1.25877863190032,-1.14957386869789,1.11134391950535));
#5582=CARTESIAN_POINT('Ctrl Pts',(1.13880944664334,-0.944305487007855,1.09884895868796));
#5583=CARTESIAN_POINT('Ctrl Pts',(0.704396841252997,-0.383656855455022,
1.05873974066059));
#5584=CARTESIAN_POINT('Ctrl Pts',(0.3194079797097,-0.0774763484135167,1.02925441368461));
#5585=CARTESIAN_POINT('Ctrl Pts',(-0.351315267230051,0.19258155683384,1.03337870280986));
#5586=CARTESIAN_POINT('Ctrl Pts',(-0.596513631217612,0.251867130809852,
1.0423383445272));
#5587=CARTESIAN_POINT('Ctrl Pts',(-1.13113472088033,0.213270370428087,1.08897889079772));
#5588=CARTESIAN_POINT('Ctrl Pts',(-1.42130583176012,0.0948756747378918,
1.12960533249102));
#5589=CARTESIAN_POINT('Ctrl Pts',(-1.83584202147282,-0.331547799152291,
1.22588454353743));
#5590=CARTESIAN_POINT('Ctrl Pts',(-1.95700322531958,-0.611665527627663,
1.277171368661));
#5591=CARTESIAN_POINT('Ctrl Pts',(-2.07819512408842,-1.242400220448,1.38178133221873));
#5592=CARTESIAN_POINT('Ctrl Pts',(-2.08276098361269,-1.6022969587106,1.43688814851895));
#5593=CARTESIAN_POINT('Ctrl Pts',(-2.03659883245755,-2.03143576587941,1.49964134391094));
#5594=CARTESIAN_POINT('Ctrl Pts',(-2.58520502693868,-0.202427724268506,
0.257988551864641));
#5595=CARTESIAN_POINT('Ctrl Pts',(-2.52286959602286,-0.0991599935411917,
0.480414187803598));
#5596=CARTESIAN_POINT('Ctrl Pts',(-2.49069703110151,-0.0547751581915275,
0.650391647036053));
#5597=CARTESIAN_POINT('Ctrl Pts',(-2.45901975307171,-0.0405967151270361,
0.860323812136826));
#5598=CARTESIAN_POINT('Ctrl Pts',(-2.45755776601418,-0.0668772768837554,
0.890888701795052));
#5599=CARTESIAN_POINT('Ctrl Pts',(-2.43814972704647,-0.0997101264501223,
0.889828411549012));
#5600=CARTESIAN_POINT('Ctrl Pts',(-2.42322436247891,-0.109485358511338,
0.880041033565627));
#5601=CARTESIAN_POINT('Ctrl Pts',(-2.39625766944769,-0.209667337073921,
0.892370624522099));
#5602=CARTESIAN_POINT('Ctrl Pts',(-2.38312298955208,-0.301090693054413,
0.900119763459602));
#5603=CARTESIAN_POINT('Ctrl Pts',(-2.32301076703839,-0.484396978702216,
0.896687786586603));
#5604=CARTESIAN_POINT('Ctrl Pts',(-2.2882208769662,-0.554099346897494,0.893755324967696));
#5605=CARTESIAN_POINT('Ctrl Pts',(-2.26024650082642,-0.688025321619785,
0.897037457090494));
#5606=CARTESIAN_POINT('Ctrl Pts',(-2.26909685245436,-0.753271393542086,
0.90056283633815));
#5607=CARTESIAN_POINT('Ctrl Pts',(-2.30562038065636,-0.958868133830514,
0.903741395119929));
#5608=CARTESIAN_POINT('Ctrl Pts',(-2.32345605900597,-1.11054614021518,0.896323357424417));
#5609=CARTESIAN_POINT('Ctrl Pts',(-2.32766903008263,-1.57324447167574,0.855513659745901));
#5610=CARTESIAN_POINT('Ctrl Pts',(-2.26534134624811,-1.89313706735396,0.802550146205944));
#5611=CARTESIAN_POINT('Ctrl Pts',(-1.8784097009876,-2.34623302779759,0.737850016479276));
#5612=CARTESIAN_POINT('Ctrl Pts',(-1.62856420025181,-2.47940372964513,0.723656709579273));
#5613=CARTESIAN_POINT('Ctrl Pts',(-1.0677159752808,-2.64815885225886,0.711821011413811));
#5614=CARTESIAN_POINT('Ctrl Pts',(-0.754654442434687,-2.68423961890214,
0.7143656987144));
#5615=CARTESIAN_POINT('Ctrl Pts',(-0.146547655379389,-2.66387954969245,
0.728109209430922));
#5616=CARTESIAN_POINT('Ctrl Pts',(0.148360185492318,-2.60647744552693,0.739290473004851));
#5617=CARTESIAN_POINT('Ctrl Pts',(0.630407318327205,-2.38898663042632,0.760041102206871));
#5618=CARTESIAN_POINT('Ctrl Pts',(0.826421854426146,-2.22824278895934,0.770653093691493));
#5619=CARTESIAN_POINT('Ctrl Pts',(0.944626927682175,-1.85585057919288,0.775558178553095));
#5620=CARTESIAN_POINT('Ctrl Pts',(0.925034692722124,-1.68883328142547,0.773222476225436));
#5621=CARTESIAN_POINT('Ctrl Pts',(0.811065913099062,-1.36506222450943,0.767306282372666));
#5622=CARTESIAN_POINT('Ctrl Pts',(0.713303855474414,-1.20565623956688,0.763081995675995));
#5623=CARTESIAN_POINT('Ctrl Pts',(0.34282900880003,-0.763013140860391,0.752549842977497));
#5624=CARTESIAN_POINT('Ctrl Pts',(-0.00364320811200702,-0.51409270041443,
0.749182852233819));
#5625=CARTESIAN_POINT('Ctrl Pts',(-0.51978409527715,-0.322125645865647,
0.768702071980997));
#5626=CARTESIAN_POINT('Ctrl Pts',(-0.692921619426966,-0.288496673462745,
0.779141999853542));
#5627=CARTESIAN_POINT('Ctrl Pts',(-1.02265615110868,-0.318050712715351,
0.812410654246396));
#5628=CARTESIAN_POINT('Ctrl Pts',(-1.17942291671907,-0.38451642598792,0.835724403097336));
#5629=CARTESIAN_POINT('Ctrl Pts',(-1.42433925564296,-0.641664631057489,
0.895455616106331));
#5630=CARTESIAN_POINT('Ctrl Pts',(-1.51197566296117,-0.828011441539482,
0.931198033441523));
#5631=CARTESIAN_POINT('Ctrl Pts',(-1.60515675444377,-1.32815869991775,1.016496711423));
#5632=CARTESIAN_POINT('Ctrl Pts',(-1.61139422048387,-1.6433989280412,1.06632932813794));
#5633=CARTESIAN_POINT('Ctrl Pts',(-1.5676596498637,-2.03832577625143,1.12541070542012));
#5634=CARTESIAN_POINT('Ctrl Pts',(-2.,-0.264726219523816,0.141138331776411));
#5635=CARTESIAN_POINT('Ctrl Pts',(-1.93317897182823,-0.140204737359338,
0.374697162628536));
#5636=CARTESIAN_POINT('Ctrl Pts',(-1.89576248628645,-0.0714193310070166,
0.563392832565318));
#5637=CARTESIAN_POINT('Ctrl Pts',(-1.85828016234107,-0.0141476745355931,
0.845995304749381));
#5638=CARTESIAN_POINT('Ctrl Pts',(-1.85721582540971,-0.0237125088868792,
0.935184056400945));
#5639=CARTESIAN_POINT('Ctrl Pts',(-1.86061638209651,-0.0666740172427863,
1.06187361715673));
#5640=CARTESIAN_POINT('Ctrl Pts',(-1.86640738686477,-0.101672715288381,
1.11012925637074));
#5641=CARTESIAN_POINT('Ctrl Pts',(-1.88833554246329,-0.235746153313808,
1.21545234876845));
#5642=CARTESIAN_POINT('Ctrl Pts',(-1.9033753276643,-0.335251316849042,1.26604967753693));
#5643=CARTESIAN_POINT('Ctrl Pts',(-1.9189176957612,-0.518726439558199,1.34035163842065));
#5644=CARTESIAN_POINT('Ctrl Pts',(-1.92137116451861,-0.585485291115871,
1.36832017615168));
#5645=CARTESIAN_POINT('Ctrl Pts',(-1.93896943688162,-0.724455435049461,
1.40322870297494));
#5646=CARTESIAN_POINT('Ctrl Pts',(-1.95325668725115,-0.796545227124419,
1.40888781048668));
#5647=CARTESIAN_POINT('Ctrl Pts',(-1.99209925627655,-1.01599260874888,1.41219882843878));
#5648=CARTESIAN_POINT('Ctrl Pts',(-2.00898122237353,-1.16761549888469,1.40420126611032));
#5649=CARTESIAN_POINT('Ctrl Pts',(-2.01271588366055,-1.60175062040053,1.36576567629003));
#5650=CARTESIAN_POINT('Ctrl Pts',(-1.95046360827934,-1.85129221142242,1.32547580954877));
#5651=CARTESIAN_POINT('Ctrl Pts',(-1.69792570410908,-2.14007513561928,1.27973035876422));
#5652=CARTESIAN_POINT('Ctrl Pts',(-1.50788517190343,-2.24578075342313,1.26508664601861));
#5653=CARTESIAN_POINT('Ctrl Pts',(-1.03351721040672,-2.37409803162741,1.24662061906772));
#5654=CARTESIAN_POINT('Ctrl Pts',(-0.753928362614793,-2.39679255199907,
1.24243205928811));
#5655=CARTESIAN_POINT('Ctrl Pts',(-0.218845999430284,-2.35785399723118,
1.24055602083421));
#5656=CARTESIAN_POINT('Ctrl Pts',(0.0368662467341799,-2.29519092886669,
1.24322556456469));
#5657=CARTESIAN_POINT('Ctrl Pts',(0.411239882065782,-2.11406967659605,1.2495991139221));
#5658=CARTESIAN_POINT('Ctrl Pts',(0.518384719875618,-2.00298884738698,1.25072899682664));
#5659=CARTESIAN_POINT('Ctrl Pts',(0.571801954928687,-1.83523605217566,1.25334679757698));
#5660=CARTESIAN_POINT('Ctrl Pts',(0.569023344394799,-1.74044478899434,1.25599881503435));
#5661=CARTESIAN_POINT('Ctrl Pts',(0.494126240428662,-1.50788563057796,1.25886663470126));
#5662=CARTESIAN_POINT('Ctrl Pts',(0.421606239831573,-1.37485017740085,1.26041038383949));
#5663=CARTESIAN_POINT('Ctrl Pts',(0.127609128452456,-0.989034614321357,
1.26907008807672));
#5664=CARTESIAN_POINT('Ctrl Pts',(-0.170570542490676,-0.751894328558357,
1.28023791867232));
#5665=CARTESIAN_POINT('Ctrl Pts',(-0.569600762546571,-0.586703644418381,
1.30640573381989));
#5666=CARTESIAN_POINT('Ctrl Pts',(-0.692371618949951,-0.563856396440986,
1.31685387723007));
#5667=CARTESIAN_POINT('Ctrl Pts',(-0.882581236630141,-0.577499841895708,
1.33968897633028));
#5668=CARTESIAN_POINT('Ctrl Pts',(-0.949730803773584,-0.6053755874494,1.35084566027416));
#5669=CARTESIAN_POINT('Ctrl Pts',(-1.08267031338154,-0.742643707380371,
1.38530535019886));
#5670=CARTESIAN_POINT('Ctrl Pts',(-1.14980571385887,-0.863823663666268,
1.41045379245241));
#5671=CARTESIAN_POINT('Ctrl Pts',(-1.22863752459304,-1.27359538565792,1.48274964800499));
#5672=CARTESIAN_POINT('Ctrl Pts',(-1.23841278692706,-1.55826711159036,1.52914339518866));
#5673=CARTESIAN_POINT('Ctrl Pts',(-1.19858468901873,-1.92998306793573,1.58589472341859));
#5674=CARTESIAN_POINT('',(-1.7123707667093,-0.0792203553185641,-0.0315207782236257));
#5675=CARTESIAN_POINT('',(-1.97217110131402,0.328135292296241,-0.0174867429177148));
#5676=CARTESIAN_POINT('Ctrl Pts',(-1.71237076670932,-0.0792203554440619,
-0.0315207779082008));
#5677=CARTESIAN_POINT('Ctrl Pts',(-1.71225680255821,-0.0788631339014023,
-0.0313786429465269));
#5678=CARTESIAN_POINT('Ctrl Pts',(-1.71208823782772,-0.0782706097349225,
-0.0313418726165944));
#5679=CARTESIAN_POINT('Ctrl Pts',(-1.71157335911718,-0.0763326226625869,
-0.0314050208455891));
#5680=CARTESIAN_POINT('Ctrl Pts',(-1.71136778606381,-0.0755433059720559,
-0.0314456176241967));
#5681=CARTESIAN_POINT('Ctrl Pts',(-1.71086177270017,-0.0735744218851083,
-0.0315527227334411));
#5682=CARTESIAN_POINT('Ctrl Pts',(-1.71050659837137,-0.0721571984421657,
-0.0316391398449165));
#5683=CARTESIAN_POINT('Ctrl Pts',(-1.70947628057217,-0.0679313170811708,
-0.0318967502239478));
#5684=CARTESIAN_POINT('Ctrl Pts',(-1.70882852767769,-0.0651327994730381,
-0.0320693383888488));
#5685=CARTESIAN_POINT('Ctrl Pts',(-1.7069794858788,-0.0566966787293398,
-0.0325751880937715));
#5686=CARTESIAN_POINT('Ctrl Pts',(-1.70587853876313,-0.0510502238207176,
-0.0328976980002992));
#5687=CARTESIAN_POINT('Ctrl Pts',(-1.70296990262491,-0.0340398585560832,
-0.0338106570223856));
#5688=CARTESIAN_POINT('Ctrl Pts',(-1.70155701975247,-0.0226075766793059,
-0.0343482598789538));
#5689=CARTESIAN_POINT('Ctrl Pts',(-1.69895448923435,0.0115451283008395,
-0.0357337044930367));
#5690=CARTESIAN_POINT('Ctrl Pts',(-1.69932902938613,0.034374979625958,-0.0363725220507445));
#5691=CARTESIAN_POINT('Ctrl Pts',(-1.70678458981123,0.100203388283196,-0.0374512675022018));
#5692=CARTESIAN_POINT('Ctrl Pts',(-1.71963219235882,0.142271280888972,-0.0371798099524647));
#5693=CARTESIAN_POINT('Ctrl Pts',(-1.75844045789029,0.212695496528277,-0.0350857448847548));
#5694=CARTESIAN_POINT('Ctrl Pts',(-1.78187136755302,0.241571788518346,-0.0335185403772877));
#5695=CARTESIAN_POINT('Ctrl Pts',(-1.8355021662325,0.286103340279215,-0.0295180509329332));
#5696=CARTESIAN_POINT('Ctrl Pts',(-1.86409005060045,0.30238404614985,-0.0272408755264394));
#5697=CARTESIAN_POINT('Ctrl Pts',(-1.91989972762967,0.321892907016035,-0.0224470229788942));
#5698=CARTESIAN_POINT('Ctrl Pts',(-1.94585998817096,0.326883504438017,-0.0200983562132771));
#5699=CARTESIAN_POINT('Ctrl Pts',(-1.97217850583874,0.328104890351764,-0.0175485997260151));
#5700=CARTESIAN_POINT('',(-1.66752387161258,-1.92309305756372,1.96012536190956));
#5701=CARTESIAN_POINT('Ctrl Pts',(-1.9721636967893,0.328165694240719,-0.0174248861094145));
#5702=CARTESIAN_POINT('Ctrl Pts',(-1.96047851223817,0.356633337001664,0.0404871888707593));
#5703=CARTESIAN_POINT('Ctrl Pts',(-1.95013077049801,0.382355896985405,0.0964727267131344));
#5704=CARTESIAN_POINT('Ctrl Pts',(-1.93177358498602,0.429073484290914,0.206103730203931));
#5705=CARTESIAN_POINT('Ctrl Pts',(-1.92380662254987,0.449981339228045,0.259693515327892));
#5706=CARTESIAN_POINT('Ctrl Pts',(-1.91012545460458,0.487292465067314,0.365429133263016));
#5707=CARTESIAN_POINT('Ctrl Pts',(-1.90447531620791,0.503564356399332,0.417500925391009));
#5708=CARTESIAN_POINT('Ctrl Pts',(-1.89652758858992,0.528274529448912,0.508776271663394));
#5709=CARTESIAN_POINT('Ctrl Pts',(-1.89377973603894,0.537635019250509,0.54842142255703));
#5710=CARTESIAN_POINT('Ctrl Pts',(-1.88054212115223,0.589499219533149,0.806948039420934));
#5711=CARTESIAN_POINT('Ctrl Pts',(-1.89355670297749,0.583239799293228,1.01230148627963));
#5712=CARTESIAN_POINT('Ctrl Pts',(-1.96699692305992,0.455902737146338,1.36395889494755));
#5713=CARTESIAN_POINT('Ctrl Pts',(-2.0260966400903,0.336426883774145,1.4995078927604));
#5714=CARTESIAN_POINT('Ctrl Pts',(-2.15596846531112,0.0612442801182847,
1.67285491314019));
#5715=CARTESIAN_POINT('Ctrl Pts',(-2.22783813535845,-0.0940322899337932,
1.71712292179187));
#5716=CARTESIAN_POINT('Ctrl Pts',(-2.33598259475191,-0.33920269686933,1.73476325774032));
#5717=CARTESIAN_POINT('Ctrl Pts',(-2.37364523276466,-0.423071247215849,
1.72904949400271));
#5718=CARTESIAN_POINT('Ctrl Pts',(-2.43018814721365,-0.596053964829743,
1.72459007815411));
#5719=CARTESIAN_POINT('Ctrl Pts',(-2.44992604374876,-0.685289715308575,
1.72712526048845));
#5720=CARTESIAN_POINT('Ctrl Pts',(-2.49822456222477,-0.958676731041413,
1.73139362094456));
#5721=CARTESIAN_POINT('Ctrl Pts',(-2.51952437158661,-1.14742069861778,1.72177264812241));
#5722=CARTESIAN_POINT('Ctrl Pts',(-2.52421524419146,-1.71230284911647,1.67203589473725));
#5723=CARTESIAN_POINT('Ctrl Pts',(-2.45059179936626,-2.09932880466486,1.60645497054434));
#5724=CARTESIAN_POINT('Ctrl Pts',(-1.98962439178456,-2.61780033767695,1.53519651937827));
#5725=CARTESIAN_POINT('Ctrl Pts',(-1.70626447510137,-2.75463798845714,1.52294419434135));
#5726=CARTESIAN_POINT('Ctrl Pts',(-1.09694793499771,-2.90941590356896,1.51900250281471));
#5727=CARTESIAN_POINT('Ctrl Pts',(-0.766252504594009,-2.92727330542218,
1.52767939121794));
#5728=CARTESIAN_POINT('Ctrl Pts',(-0.128899912590115,-2.86525349144335,
1.55261884723468));
#5729=CARTESIAN_POINT('Ctrl Pts',(0.177538775386479,-2.78640624113666,1.56852441648561));
#5730=CARTESIAN_POINT('Ctrl Pts',(0.694316196436972,-2.52237373057128,1.59609027963019));
#5731=CARTESIAN_POINT('Ctrl Pts',(0.916171749283459,-2.32981104713974,1.610324720381));
#5732=CARTESIAN_POINT('Ctrl Pts',(1.06563235049552,-1.86355969472817,1.61635239083565));
#5733=CARTESIAN_POINT('Ctrl Pts',(1.05129988764842,-1.66506108797555,1.61232780975798));
#5734=CARTESIAN_POINT('Ctrl Pts',(0.941838959229918,-1.29239727476634,1.60290427183405));
#5735=CARTESIAN_POINT('Ctrl Pts',(0.847111831000521,-1.11349942484178,1.59617734685152));
#5736=CARTESIAN_POINT('Ctrl Pts',(0.48917696090542,-0.609678328916015,1.57525998575985));
#5737=CARTESIAN_POINT('Ctrl Pts',(0.152480645331013,-0.315277976557456,
1.560309480123));
#5738=CARTESIAN_POINT('Ctrl Pts',(-0.401131934499452,-0.0719964417188535,
1.57108236464872));
#5739=CARTESIAN_POINT('Ctrl Pts',(-0.5959636307406,-0.0234925921684045,
1.58005022190368));
#5740=CARTESIAN_POINT('Ctrl Pts',(-0.99105980640179,-0.0461787587522702,
1.61625721288154));
#5741=CARTESIAN_POINT('Ctrl Pts',(-1.19161371881466,-0.12598348672354,1.64472658966789));
#5742=CARTESIAN_POINT('Ctrl Pts',(-1.49417307921139,-0.432526875475132,
1.71573427762991));
#5743=CARTESIAN_POINT('Ctrl Pts',(-1.5948332762173,-0.647477749754412,1.75642712767188));
#5744=CARTESIAN_POINT('Ctrl Pts',(-1.70167589423767,-1.18783690618816,1.84803426880073));
#5745=CARTESIAN_POINT('Ctrl Pts',(-1.70977955005582,-1.5171651422599,1.89970221556995));
#5746=CARTESIAN_POINT('Ctrl Pts',(-1.66752387161256,-1.92309305756368,1.96012536190953));
#5747=CARTESIAN_POINT('',(-1.19858468901873,-1.92998306793576,1.58589472341869));
#5748=CARTESIAN_POINT('Origin',(-1.43305428031565,-1.92653806274973,1.77301004266414));
#5749=CARTESIAN_POINT('',(-2.,-0.264726219523809,0.141138331776429));
#5750=CARTESIAN_POINT('Ctrl Pts',(-2.,-0.264726219523809,0.141138331776429));
#5751=CARTESIAN_POINT('Ctrl Pts',(-1.93317897182823,-0.140204737359338,
0.374697162628536));
#5752=CARTESIAN_POINT('Ctrl Pts',(-1.89576248628645,-0.0714193310070166,
0.563392832565318));
#5753=CARTESIAN_POINT('Ctrl Pts',(-1.85828016234107,-0.0141476745355931,
0.845995304749381));
#5754=CARTESIAN_POINT('Ctrl Pts',(-1.85721582540971,-0.0237125088868792,
0.935184056400945));
#5755=CARTESIAN_POINT('Ctrl Pts',(-1.86061638209651,-0.0666740172427863,
1.06187361715673));
#5756=CARTESIAN_POINT('Ctrl Pts',(-1.86640738686477,-0.101672715288381,
1.11012925637074));
#5757=CARTESIAN_POINT('Ctrl Pts',(-1.88833554246329,-0.235746153313808,
1.21545234876845));
#5758=CARTESIAN_POINT('Ctrl Pts',(-1.9033753276643,-0.335251316849042,1.26604967753693));
#5759=CARTESIAN_POINT('Ctrl Pts',(-1.9189176957612,-0.518726439558199,1.34035163842065));
#5760=CARTESIAN_POINT('Ctrl Pts',(-1.92137116451861,-0.585485291115871,
1.36832017615168));
#5761=CARTESIAN_POINT('Ctrl Pts',(-1.93896943688162,-0.724455435049461,
1.40322870297494));
#5762=CARTESIAN_POINT('Ctrl Pts',(-1.95325668725115,-0.796545227124419,
1.40888781048668));
#5763=CARTESIAN_POINT('Ctrl Pts',(-1.99209925627655,-1.01599260874888,1.41219882843878));
#5764=CARTESIAN_POINT('Ctrl Pts',(-2.00898122237353,-1.16761549888469,1.40420126611032));
#5765=CARTESIAN_POINT('Ctrl Pts',(-2.01271588366055,-1.60175062040053,1.36576567629003));
#5766=CARTESIAN_POINT('Ctrl Pts',(-1.95046360827934,-1.85129221142242,1.32547580954877));
#5767=CARTESIAN_POINT('Ctrl Pts',(-1.69792570410908,-2.14007513561928,1.27973035876422));
#5768=CARTESIAN_POINT('Ctrl Pts',(-1.50788517190343,-2.24578075342313,1.26508664601861));
#5769=CARTESIAN_POINT('Ctrl Pts',(-1.03351721040672,-2.37409803162741,1.24662061906772));
#5770=CARTESIAN_POINT('Ctrl Pts',(-0.753928362614793,-2.39679255199907,
1.24243205928811));
#5771=CARTESIAN_POINT('Ctrl Pts',(-0.218845999430284,-2.35785399723118,
1.24055602083421));
#5772=CARTESIAN_POINT('Ctrl Pts',(0.0368662467341799,-2.29519092886669,
1.24322556456469));
#5773=CARTESIAN_POINT('Ctrl Pts',(0.411239882065782,-2.11406967659605,1.2495991139221));
#5774=CARTESIAN_POINT('Ctrl Pts',(0.518384719875618,-2.00298884738698,1.25072899682664));
#5775=CARTESIAN_POINT('Ctrl Pts',(0.571801954928687,-1.83523605217566,1.25334679757698));
#5776=CARTESIAN_POINT('Ctrl Pts',(0.569023344394799,-1.74044478899434,1.25599881503435));
#5777=CARTESIAN_POINT('Ctrl Pts',(0.494126240428662,-1.50788563057796,1.25886663470126));
#5778=CARTESIAN_POINT('Ctrl Pts',(0.421606239831573,-1.37485017740085,1.26041038383949));
#5779=CARTESIAN_POINT('Ctrl Pts',(0.127609128452456,-0.989034614321357,
1.26907008807672));
#5780=CARTESIAN_POINT('Ctrl Pts',(-0.170570542490676,-0.751894328558357,
1.28023791867232));
#5781=CARTESIAN_POINT('Ctrl Pts',(-0.569600762546571,-0.586703644418381,
1.30640573381989));
#5782=CARTESIAN_POINT('Ctrl Pts',(-0.692371618949951,-0.563856396440986,
1.31685387723007));
#5783=CARTESIAN_POINT('Ctrl Pts',(-0.882581236630141,-0.577499841895708,
1.33968897633028));
#5784=CARTESIAN_POINT('Ctrl Pts',(-0.949730803773584,-0.6053755874494,1.35084566027416));
#5785=CARTESIAN_POINT('Ctrl Pts',(-1.08267031338154,-0.742643707380371,
1.38530535019886));
#5786=CARTESIAN_POINT('Ctrl Pts',(-1.14980571385887,-0.863823663666268,
1.41045379245241));
#5787=CARTESIAN_POINT('Ctrl Pts',(-1.22863752459304,-1.27359538565792,1.48274964800499));
#5788=CARTESIAN_POINT('Ctrl Pts',(-1.23841278692706,-1.55826711159036,1.52914339518866));
#5789=CARTESIAN_POINT('Ctrl Pts',(-1.19858468901873,-1.92998306793576,1.58589472341869));
#5790=CARTESIAN_POINT('Origin',(-2.,-2.08166817117217E-14,-3.46944695195361E-14));
#5791=CARTESIAN_POINT('Ctrl Pts',(-2.00006370137914,0.278745603789511,0.110909351770506));
#5792=CARTESIAN_POINT('Ctrl Pts',(-2.02978177261913,0.487078937122742,-0.425006101824765));
#5793=CARTESIAN_POINT('Ctrl Pts',(-1.78756065046676,0.695412270456132,-0.903981534539017));
#5794=CARTESIAN_POINT('Ctrl Pts',(-1.5453395283144,0.903745603789377,-1.38295696725319));
#5795=CARTESIAN_POINT('Ctrl Pts',(-1.09608216684017,1.11207893712281,-1.67665129869622));
#5796=CARTESIAN_POINT('Ctrl Pts',(-0.646824805365941,1.32041227045615,-1.97034563013915));
#5797=CARTESIAN_POINT('Ctrl Pts',(-0.110909351770586,1.52874560378948,-2.00006370137914));
#5798=CARTESIAN_POINT('Ctrl Pts',(0.425006101824744,1.73707893712275,-2.02978177261916));
#5799=CARTESIAN_POINT('Ctrl Pts',(0.903981534538964,1.94541227045615,-1.78756065046677));
#5800=CARTESIAN_POINT('Ctrl Pts',(1.38295696725319,2.15374560378948,-1.5453395283144));
#5801=CARTESIAN_POINT('Ctrl Pts',(1.67665129869617,2.36207893712281,-1.09608216684018));
#5802=CARTESIAN_POINT('Ctrl Pts',(1.97034563013914,2.57041227045613,-0.646824805365955));
#5803=CARTESIAN_POINT('Ctrl Pts',(2.00006370137916,2.77874560378949,-0.110909351770603));
#5804=CARTESIAN_POINT('Ctrl Pts',(2.02978177261913,2.98707893712281,0.425006101824722));
#5805=CARTESIAN_POINT('Ctrl Pts',(1.78756065046677,3.19541227045615,0.903981534538913));
#5806=CARTESIAN_POINT('Ctrl Pts',(1.5453395283144,3.40374560378943,1.38295696725317));
#5807=CARTESIAN_POINT('Ctrl Pts',(1.09608216684017,3.61207893712282,1.67665129869616));
#5808=CARTESIAN_POINT('Ctrl Pts',(0.646824805365943,3.8204122704561,1.97034563013913));
#5809=CARTESIAN_POINT('Ctrl Pts',(0.1109093517706,4.02874560378949,2.00006370137908));
#5810=CARTESIAN_POINT('Ctrl Pts',(-0.425006101824727,4.23707893712277,2.02978177261911));
#5811=CARTESIAN_POINT('Ctrl Pts',(-0.903981534538964,4.44541227045615,1.78756065046676));
#5812=CARTESIAN_POINT('Ctrl Pts',(-1.38295696725319,4.65374560378948,1.54533952831435));
#5813=CARTESIAN_POINT('Ctrl Pts',(-1.67665129869618,4.86207893712285,1.09608216684011));
#5814=CARTESIAN_POINT('Ctrl Pts',(-1.97034563013914,5.07041227045609,0.646824805365927));
#5815=CARTESIAN_POINT('Ctrl Pts',(-2.00006370137914,5.27874560378947,0.110909351770506));
#5816=CARTESIAN_POINT('Ctrl Pts',(-2.02978177261913,5.48707893712276,-0.425006101824808));
#5817=CARTESIAN_POINT('Ctrl Pts',(-1.78756065046676,5.69541227045614,-0.903981534539017));
#5818=CARTESIAN_POINT('Ctrl Pts',(-1.5453395283144,5.90374560378943,-1.38295696725317));
#5819=CARTESIAN_POINT('Ctrl Pts',(-1.09608216684016,6.11207893712282,-1.67665129869616));
#5820=CARTESIAN_POINT('Ctrl Pts',(-0.646824805365928,6.32041227045614,-1.97034563013915));
#5821=CARTESIAN_POINT('Ctrl Pts',(-0.110909351770598,6.52874560378952,-2.00006370137919));
#5822=CARTESIAN_POINT('Ctrl Pts',(0.425006101824742,6.73707893712276,-2.02978177261914));
#5823=CARTESIAN_POINT('Ctrl Pts',(0.903981534538965,6.94541227045619,-1.78756065046677));
#5824=CARTESIAN_POINT('Ctrl Pts',(1.3829569672532,7.15374560378946,-1.54533952831446));
#5825=CARTESIAN_POINT('Ctrl Pts',(1.67665129869614,7.36207893712281,-1.09608216684023));
#5826=CARTESIAN_POINT('Ctrl Pts',(1.97034563013915,7.57041227045615,-0.646824805365941));
#5827=CARTESIAN_POINT('Ctrl Pts',(2.00006370137914,7.77874560378953,-0.11090935177061));
#5828=CARTESIAN_POINT('Ctrl Pts',(2.02978177261913,7.98707893712276,0.425006101824722));
#5829=CARTESIAN_POINT('Ctrl Pts',(1.78756065046677,8.19541227045616,0.903981534538955));
#5830=CARTESIAN_POINT('Ctrl Pts',(1.54533952831442,8.40374560378946,1.38295696725319));
#5831=CARTESIAN_POINT('Ctrl Pts',(1.09608216684017,8.61207893712284,1.67665129869611));
#5832=CARTESIAN_POINT('Ctrl Pts',(0.646824805365943,8.82041227045615,1.97034563013914));
#5833=CARTESIAN_POINT('Ctrl Pts',(0.110909351770597,9.0287456037895,2.00006370137908));
#5834=CARTESIAN_POINT('Ctrl Pts',(-0.42500610182474,9.23707893712282,2.02978177261913));
#5835=CARTESIAN_POINT('Ctrl Pts',(-0.903981534538962,9.44541227045615,1.78756065046671));
#5836=CARTESIAN_POINT('Ctrl Pts',(-1.38295696725319,9.65374560378948,1.5453395283144));
#5837=CARTESIAN_POINT('Ctrl Pts',(-1.67665129869616,9.86207893712282,1.09608216684017));
#5838=CARTESIAN_POINT('Ctrl Pts',(-1.97034563013914,10.0704122704562,0.646824805365941));
#5839=CARTESIAN_POINT('Ctrl Pts',(-2.00006370137912,10.2787456037895,0.110909351770534));
#5840=CARTESIAN_POINT('Ctrl Pts',(-2.02978177261913,10.4870789371228,-0.425006101824744));
#5841=CARTESIAN_POINT('Ctrl Pts',(-1.78756065046676,10.6954122704562,-0.903981534539066));
#5842=CARTESIAN_POINT('Ctrl Pts',(-1.5453395283144,10.9037456037894,-1.3829569672532));
#5843=CARTESIAN_POINT('Ctrl Pts',(-1.09608216684017,11.1120789371228,-1.67665129869622));
#5844=CARTESIAN_POINT('Ctrl Pts',(-0.646824805365941,11.3204122704561,-1.97034563013915));
#5845=CARTESIAN_POINT('Ctrl Pts',(-0.1109093517706,11.5287456037895,-2.00006370137916));
#5846=CARTESIAN_POINT('Ctrl Pts',(0.425006101824742,11.7370789371228,-2.02978177261915));
#5847=CARTESIAN_POINT('Ctrl Pts',(0.903981534538964,11.9454122704562,-1.78756065046677));
#5848=CARTESIAN_POINT('Ctrl Pts',(1.38295696725319,12.1537456037895,-1.54533952831446));
#5849=CARTESIAN_POINT('Ctrl Pts',(1.67665129869616,12.3620789371228,-1.09608216684018));
#5850=CARTESIAN_POINT('Ctrl Pts',(1.97034563013917,12.5704122704561,-0.646824805365955));
#5851=CARTESIAN_POINT('Ctrl Pts',(2.00006370137914,12.7787456037895,-0.110909351770652));
#5852=CARTESIAN_POINT('Ctrl Pts',(2.02978177261913,12.9870789371228,0.425006101824744));
#5853=CARTESIAN_POINT('Ctrl Pts',(1.78756065046676,13.1954122704562,0.903981534538906));
#5854=CARTESIAN_POINT('Ctrl Pts',(1.5453395283144,13.4037456037895,1.38295696725318));
#5855=CARTESIAN_POINT('Ctrl Pts',(1.09608216684017,13.6120789371228,1.67665129869616));
#5856=CARTESIAN_POINT('Ctrl Pts',(0.646824805365943,13.8204122704562,1.97034563013915));
#5857=CARTESIAN_POINT('Ctrl Pts',(0.1109093517706,14.0287456037895,2.0000637013791));
#5858=CARTESIAN_POINT('Ctrl Pts',(-0.425006101824742,14.2370789371228,2.02978177261913));
#5859=CARTESIAN_POINT('Ctrl Pts',(-0.903981534538964,14.4454122704562,1.78756065046667));
#5860=CARTESIAN_POINT('Ctrl Pts',(-1.38295696725319,14.6537456037895,1.54533952831435));
#5861=CARTESIAN_POINT('Ctrl Pts',(-1.67665129869616,14.8620789371229,1.09608216684011));
#5862=CARTESIAN_POINT('Ctrl Pts',(-1.97034563013913,15.0704122704562,0.646824805365955));
#5863=CARTESIAN_POINT('Ctrl Pts',(-2.00006370137914,15.2787456037895,0.110909351770541));
#5864=CARTESIAN_POINT('Ctrl Pts',(-2.02978177261913,15.4870789371228,-0.425006101824851));
#5865=CARTESIAN_POINT('Ctrl Pts',(-1.78756065046676,15.6954122704562,-0.903981534538976));
#5866=CARTESIAN_POINT('Ctrl Pts',(-1.5453395283144,15.9037456037895,-1.38295696725319));
#5867=CARTESIAN_POINT('Ctrl Pts',(-1.09608216684016,16.1120789371229,-1.6766512986962));
#5868=CARTESIAN_POINT('Ctrl Pts',(-0.646824805365941,16.3204122704561,-1.9703456301392));
#5869=CARTESIAN_POINT('Ctrl Pts',(-0.1109093517706,16.5287456037895,-2.00006370137919));
#5870=CARTESIAN_POINT('Ctrl Pts',(0.425006101824744,16.7370789371228,-2.02978177261913));
#5871=CARTESIAN_POINT('Ctrl Pts',(0.903981534538977,16.9454122704562,-1.78756065046677));
#5872=CARTESIAN_POINT('Ctrl Pts',(1.38295696725319,17.1537456037895,-1.5453395283144));
#5873=CARTESIAN_POINT('Ctrl Pts',(1.67665129869616,17.3620789371229,-1.09608216684022));
#5874=CARTESIAN_POINT('Ctrl Pts',(1.97034563013914,17.5704122704561,-0.646824805365941));
#5875=CARTESIAN_POINT('Ctrl Pts',(2.00006370137914,17.7787456037895,-0.11090935177061));
#5876=CARTESIAN_POINT('Ctrl Pts',(2.02978177261913,17.9870789371228,0.425006101824686));
#5877=CARTESIAN_POINT('Ctrl Pts',(1.78756065046677,18.1954122704562,0.903981534538948));
#5878=CARTESIAN_POINT('Ctrl Pts',(1.54533952831442,18.4037456037895,1.38295696725319));
#5879=CARTESIAN_POINT('Ctrl Pts',(1.09608216684017,18.6120789371228,1.67665129869611));
#5880=CARTESIAN_POINT('Ctrl Pts',(0.646824805365943,18.8204122704562,1.97034563013914));
#5881=CARTESIAN_POINT('Ctrl Pts',(0.110909351770598,19.0287456037895,2.00006370137909));
#5882=CARTESIAN_POINT('Ctrl Pts',(-0.425006101824742,19.2370789371228,2.02978177261913));
#5883=CARTESIAN_POINT('Ctrl Pts',(-0.903981534538962,19.4454122704562,1.78756065046669));
#5884=CARTESIAN_POINT('Ctrl Pts',(-1.38295696725319,19.6537456037895,1.5453395283144));
#5885=CARTESIAN_POINT('Ctrl Pts',(-1.67665129869616,19.8620789371228,1.09608216684013));
#5886=CARTESIAN_POINT('Ctrl Pts',(-1.97034563013915,20.0704122704561,0.646824805365941));
#5887=CARTESIAN_POINT('Ctrl Pts',(-2.00006370137912,20.2787456037895,0.110909351770513));
#5888=CARTESIAN_POINT('Ctrl Pts',(-2.02978177261911,20.4870789371228,-0.425006101824801));
#5889=CARTESIAN_POINT('Ctrl Pts',(-1.78756065046676,20.6954122704562,-0.903981534539024));
#5890=CARTESIAN_POINT('Ctrl Pts',(-1.54533952831439,20.9037456037895,-1.38295696725322));
#5891=CARTESIAN_POINT('Ctrl Pts',(-1.09608216684018,21.1120789371229,-1.67665129869622));
#5892=CARTESIAN_POINT('Ctrl Pts',(-0.646824805365943,21.3204122704561,-1.97034563013915));
#5893=CARTESIAN_POINT('Ctrl Pts',(-0.1109093517706,21.5287456037895,-2.00006370137914));
#5894=CARTESIAN_POINT('Ctrl Pts',(0.425006101824742,21.7370789371228,-2.02978177261912));
#5895=CARTESIAN_POINT('Ctrl Pts',(0.903981534538964,21.9454122704562,-1.7875606504668));
#5896=CARTESIAN_POINT('Ctrl Pts',(1.38295696725319,22.1537456037895,-1.54533952831446));
#5897=CARTESIAN_POINT('Ctrl Pts',(1.67665129869617,22.3620789371229,-1.09608216684019));
#5898=CARTESIAN_POINT('Ctrl Pts',(1.97034563013912,22.5704122704561,-0.646824805365941));
#5899=CARTESIAN_POINT('Ctrl Pts',(2.00006370137914,22.7787456037895,-0.110909351770638));
#5900=CARTESIAN_POINT('Ctrl Pts',(2.02978177261915,22.9870789371228,0.425006101824744));
#5901=CARTESIAN_POINT('Ctrl Pts',(1.78756065046677,23.1954122704562,0.903981534538906));
#5902=CARTESIAN_POINT('Ctrl Pts',(1.5453395283144,23.4037456037895,1.38295696725318));
#5903=CARTESIAN_POINT('Ctrl Pts',(1.09608216684017,23.6120789371229,1.67665129869614));
#5904=CARTESIAN_POINT('Ctrl Pts',(0.646824805365957,23.8204122704561,1.97034563013915));
#5905=CARTESIAN_POINT('Ctrl Pts',(0.1109093517706,24.0287456037895,2.00006370137905));
#5906=CARTESIAN_POINT('Ctrl Pts',(-0.425006101824742,24.2370789371228,2.02978177261914));
#5907=CARTESIAN_POINT('Ctrl Pts',(-0.903981534538964,24.4454122704562,1.78756065046667));
#5908=CARTESIAN_POINT('Ctrl Pts',(-1.38295696725317,24.6537456037895,1.54533952831433));
#5909=CARTESIAN_POINT('Ctrl Pts',(-1.67665129869615,24.8620789371229,1.09608216684012));
#5910=CARTESIAN_POINT('Ctrl Pts',(-1.97034563013914,25.0704122704562,0.646824805365955));
#5911=CARTESIAN_POINT('Ctrl Pts',(-2.00006370137914,25.2787456037895,0.110909351770548));
#5912=CARTESIAN_POINT('Ctrl Pts',(-2.02978177261913,25.4870789371228,-0.425006101824772));
#5913=CARTESIAN_POINT('Ctrl Pts',(-1.78756065046676,25.6954122704562,-0.903981534538976));
#5914=CARTESIAN_POINT('Ctrl Pts',(-1.5453395283144,25.9037456037895,-1.38295696725319));
#5915=CARTESIAN_POINT('Ctrl Pts',(-1.09608216684017,26.1120789371229,-1.67665129869619));
#5916=CARTESIAN_POINT('Ctrl Pts',(-0.646824805365941,26.3204122704561,-1.9703456301392));
#5917=CARTESIAN_POINT('Ctrl Pts',(-0.1109093517706,26.5287456037895,-2.00006370137917));
#5918=CARTESIAN_POINT('Ctrl Pts',(0.425006101824756,26.7370789371228,-2.02978177261913));
#5919=CARTESIAN_POINT('Ctrl Pts',(0.903981534538977,26.9454122704562,-1.78756065046682));
#5920=CARTESIAN_POINT('Ctrl Pts',(1.38295696725319,27.1537456037895,-1.5453395283144));
#5921=CARTESIAN_POINT('Ctrl Pts',(1.67665129869614,27.3620789371229,-1.09608216684021));
#5922=CARTESIAN_POINT('Ctrl Pts',(1.97034563013914,27.5704122704562,-0.646824805365969));
#5923=CARTESIAN_POINT('Ctrl Pts',(2.00006370137911,27.7787456037896,-0.110909351770603));
#5924=CARTESIAN_POINT('Ctrl Pts',(2.02978177261913,27.9870789371228,0.425006101824736));
#5925=CARTESIAN_POINT('Ctrl Pts',(1.78756065046677,28.1954122704562,0.903981534538934));
#5926=CARTESIAN_POINT('Ctrl Pts',(1.54533952831439,28.4037456037895,1.38295696725318));
#5927=CARTESIAN_POINT('Ctrl Pts',(1.09608216684017,28.6120789371229,1.67665129869612));
#5928=CARTESIAN_POINT('Ctrl Pts',(0.646824805365943,28.8204122704562,1.97034563013911));
#5929=CARTESIAN_POINT('Ctrl Pts',(0.110909351770614,29.0287456037896,2.0000637013791));
#5930=CARTESIAN_POINT('Ctrl Pts',(-0.425006101824742,29.2370789371228,2.02978177261913));
#5931=CARTESIAN_POINT('Ctrl Pts',(-0.903981534538962,29.4454122704562,1.78756065046671));
#5932=CARTESIAN_POINT('Ctrl Pts',(-1.38295696725319,29.6537456037896,1.54533952831437));
#5933=CARTESIAN_POINT('Ctrl Pts',(-1.67665129869616,29.8620789371229,1.0960821668401));
#5934=CARTESIAN_POINT('Ctrl Pts',(-1.97034563013914,30.0704122704562,0.646824805365912));
#5935=CARTESIAN_POINT('Ctrl Pts',(-2.00006370137914,30.2787456037896,0.110909351770527));
#5936=CARTESIAN_POINT('Ctrl Pts',(-2.02978177261913,30.4870789371228,-0.425006101824801));
#5937=CARTESIAN_POINT('Ctrl Pts',(-1.78756065046675,30.6954122704562,-0.90398153453901));
#5938=CARTESIAN_POINT('Ctrl Pts',(-1.5453395283144,30.9037456037895,-1.38295696725315));
#5939=CARTESIAN_POINT('Ctrl Pts',(-1.09608216684017,31.1120789371229,-1.67665129869622));
#5940=CARTESIAN_POINT('Ctrl Pts',(-0.646824805365941,31.3204122704562,-1.97034563013915));
#5941=CARTESIAN_POINT('Ctrl Pts',(-0.110909351770598,31.5287456037896,-2.00006370137914));
#5942=CARTESIAN_POINT('Ctrl Pts',(0.425006101824744,31.7370789371229,-2.02978177261914));
#5943=CARTESIAN_POINT('Ctrl Pts',(0.903981534538951,31.9454122704562,-1.78756065046679));
#5944=CARTESIAN_POINT('Ctrl Pts',(1.38295696725319,32.1537456037895,-1.54533952831446));
#5945=CARTESIAN_POINT('Ctrl Pts',(1.67665129869616,32.3620789371229,-1.09608216684022));
#5946=CARTESIAN_POINT('Ctrl Pts',(1.97034563013914,32.5704122704561,-0.646824805365941));
#5947=CARTESIAN_POINT('Ctrl Pts',(2.00006370137914,32.7787456037896,-0.11090935177061));
#5948=CARTESIAN_POINT('Ctrl Pts',(2.02978177261913,32.9870789371229,0.425006101824715));
#5949=CARTESIAN_POINT('Ctrl Pts',(1.78756065046676,33.1954122704563,0.903981534538906));
#5950=CARTESIAN_POINT('Ctrl Pts',(1.5453395283144,33.4037456037895,1.3829569672532));
#5951=CARTESIAN_POINT('Ctrl Pts',(1.09608216684017,33.6120789371229,1.67665129869615));
#5952=CARTESIAN_POINT('Ctrl Pts',(0.646824805365943,33.8204122704562,1.97034563013915));
#5953=CARTESIAN_POINT('Ctrl Pts',(0.1109093517706,34.0287456037896,2.00006370137906));
#5954=CARTESIAN_POINT('Ctrl Pts',(-0.425006101824742,34.2370789371229,2.02978177261912));
#5955=CARTESIAN_POINT('Ctrl Pts',(-0.903981534538964,34.4454122704562,1.7875606504667));
#5956=CARTESIAN_POINT('Ctrl Pts',(-1.3829569672532,34.6537456037895,1.54533952831438));
#5957=CARTESIAN_POINT('Ctrl Pts',(-1.67665129869615,34.8620789371228,1.09608216684013));
#5958=CARTESIAN_POINT('Ctrl Pts',(-1.97034563013914,35.0704122704562,0.646824805365955));
#5959=CARTESIAN_POINT('Ctrl Pts',(-2.00006370137914,35.2787456037896,0.110909351770548));
#5960=CARTESIAN_POINT('Ctrl Pts',(-2.02978177261913,35.4870789371229,-0.425006101824787));
#5961=CARTESIAN_POINT('Ctrl Pts',(-1.78756065046676,35.6954122704562,-0.903981534538996));
#5962=CARTESIAN_POINT('Ctrl Pts',(-1.5453395283144,35.9037456037895,-1.3829569672532));
#5963=CARTESIAN_POINT('Ctrl Pts',(-1.09608216684017,36.1120789371229,-1.67665129869619));
#5964=CARTESIAN_POINT('Ctrl Pts',(-0.646824805365928,36.3204122704562,-1.97034563013915));
#5965=CARTESIAN_POINT('Ctrl Pts',(-0.1109093517706,36.5287456037896,-2.00006370137918));
#5966=CARTESIAN_POINT('Ctrl Pts',(0.425006101824742,36.7370789371229,-2.02978177261914));
#5967=CARTESIAN_POINT('Ctrl Pts',(0.903981534538964,36.9454122704562,-1.78756065046682));
#5968=CARTESIAN_POINT('Ctrl Pts',(1.38295696725319,37.1537456037895,-1.5453395283144));
#5969=CARTESIAN_POINT('Ctrl Pts',(1.67665129869617,37.3620789371229,-1.09608216684022));
#5970=CARTESIAN_POINT('Ctrl Pts',(1.97034563013915,37.5704122704562,-0.646824805365941));
#5971=CARTESIAN_POINT('Ctrl Pts',(2.00006370137914,37.7787456037895,-0.110909351770645));
#5972=CARTESIAN_POINT('Ctrl Pts',(2.02978177261915,37.9870789371229,0.425006101824736));
#5973=CARTESIAN_POINT('Ctrl Pts',(1.78756065046677,38.1954122704563,0.90398153453892));
#5974=CARTESIAN_POINT('Ctrl Pts',(1.5453395283144,38.4037456037895,1.38295696725319));
#5975=CARTESIAN_POINT('Ctrl Pts',(1.09608216684019,38.6120789371229,1.67665129869612));
#5976=CARTESIAN_POINT('Ctrl Pts',(0.646824805365943,38.8204122704562,1.97034563013916));
#5977=CARTESIAN_POINT('Ctrl Pts',(0.110909351770614,39.0287456037896,2.0000637013791));
#5978=CARTESIAN_POINT('Ctrl Pts',(-0.425006101824727,39.2370789371229,2.02978177261914));
#5979=CARTESIAN_POINT('Ctrl Pts',(-0.90398153453895,39.4454122704563,1.78756065046672));
#5980=CARTESIAN_POINT('Ctrl Pts',(-1.38295696725319,39.6537456037896,1.54533952831436));
#5981=CARTESIAN_POINT('Ctrl Pts',(-1.67665129869616,39.8620789371229,1.09608216684011));
#5982=CARTESIAN_POINT('Ctrl Pts',(-1.97034563013914,40.0704122704562,0.646824805365955));
#5983=CARTESIAN_POINT('Ctrl Pts',(-2.00006370137914,40.2787456037896,0.110909351770527));
#5984=CARTESIAN_POINT('Ctrl Pts',(-2.00004246683501,0.278745607978964,0.110909353437437));
#5985=CARTESIAN_POINT('Ctrl Pts',(-2.02976053852165,0.487078941312195,-0.425000410378884));
#5986=CARTESIAN_POINT('Ctrl Pts',(-1.78754226164558,0.695412274645584,-0.903970915823348));
#5987=CARTESIAN_POINT('Ctrl Pts',(-1.5453239847695,0.903745607978829,-1.38294142126773));
#5988=CARTESIAN_POINT('Ctrl Pts',(-1.09607155101171,1.11207894131226,-1.6766329082081));
#5989=CARTESIAN_POINT('Ctrl Pts',(-0.64681911725392,1.32041227464561,-1.97032439514837));
#5990=CARTESIAN_POINT('Ctrl Pts',(-0.110909353437516,1.52874560797894,-2.00004246683502));
#5991=CARTESIAN_POINT('Ctrl Pts',(0.425000410378862,1.7370789413122,-2.02976053852169));
#5992=CARTESIAN_POINT('Ctrl Pts',(0.903970915823295,1.94541227464561,-1.78754226164558));
#5993=CARTESIAN_POINT('Ctrl Pts',(1.38294142126773,2.15374560797893,-1.5453239847695));
#5994=CARTESIAN_POINT('Ctrl Pts',(1.67663290820805,2.36207894131226,-1.09607155101172));
#5995=CARTESIAN_POINT('Ctrl Pts',(1.97032439514836,2.57041227464558,-0.646819117253935));
#5996=CARTESIAN_POINT('Ctrl Pts',(2.00004246683503,2.77874560797894,-0.110909353437534));
#5997=CARTESIAN_POINT('Ctrl Pts',(2.02976053852165,2.98707894131226,0.42500041037884));
#5998=CARTESIAN_POINT('Ctrl Pts',(1.78754226164558,3.1954122746456,0.903970915823244));
#5999=CARTESIAN_POINT('Ctrl Pts',(1.5453239847695,3.40374560797888,1.38294142126772));
#6000=CARTESIAN_POINT('Ctrl Pts',(1.09607155101171,3.61207894131227,1.67663290820804));
#6001=CARTESIAN_POINT('Ctrl Pts',(0.646819117253922,3.82041227464555,1.97032439514834));
#6002=CARTESIAN_POINT('Ctrl Pts',(0.11090935343753,4.02874560797894,2.00004246683495));
#6003=CARTESIAN_POINT('Ctrl Pts',(-0.425000410378846,4.23707894131222,2.02976053852163));
#6004=CARTESIAN_POINT('Ctrl Pts',(-0.903970915823295,4.4454122746456,1.78754226164557));
#6005=CARTESIAN_POINT('Ctrl Pts',(-1.38294142126773,4.65374560797893,1.54532398476945));
#6006=CARTESIAN_POINT('Ctrl Pts',(-1.67663290820806,4.8620789413123,1.09607155101165));
#6007=CARTESIAN_POINT('Ctrl Pts',(-1.97032439514836,5.07041227464555,0.646819117253906));
#6008=CARTESIAN_POINT('Ctrl Pts',(-2.00004246683501,5.27874560797892,0.110909353437437));
#6009=CARTESIAN_POINT('Ctrl Pts',(-2.02976053852165,5.48707894131221,-0.425000410378927));
#6010=CARTESIAN_POINT('Ctrl Pts',(-1.78754226164558,5.6954122746456,-0.903970915823348));
#6011=CARTESIAN_POINT('Ctrl Pts',(-1.5453239847695,5.90374560797888,-1.38294142126772));
#6012=CARTESIAN_POINT('Ctrl Pts',(-1.0960715510117,6.11207894131227,-1.67663290820805));
#6013=CARTESIAN_POINT('Ctrl Pts',(-0.646819117253907,6.3204122746456,-1.97032439514837));
#6014=CARTESIAN_POINT('Ctrl Pts',(-0.110909353437529,6.52874560797897,-2.00004246683506));
#6015=CARTESIAN_POINT('Ctrl Pts',(0.42500041037886,6.73707894131221,-2.02976053852166));
#6016=CARTESIAN_POINT('Ctrl Pts',(0.903970915823297,6.94541227464564,-1.78754226164558));
#6017=CARTESIAN_POINT('Ctrl Pts',(1.38294142126774,7.15374560797891,-1.54532398476956));
#6018=CARTESIAN_POINT('Ctrl Pts',(1.67663290820802,7.36207894131227,-1.09607155101177));
#6019=CARTESIAN_POINT('Ctrl Pts',(1.97032439514836,7.5704122746456,-0.64681911725392));
#6020=CARTESIAN_POINT('Ctrl Pts',(2.00004246683501,7.77874560797898,-0.110909353437541));
#6021=CARTESIAN_POINT('Ctrl Pts',(2.02976053852165,7.98707894131222,0.42500041037884));
#6022=CARTESIAN_POINT('Ctrl Pts',(1.78754226164558,8.19541227464561,0.903970915823286));
#6023=CARTESIAN_POINT('Ctrl Pts',(1.54532398476952,8.40374560797891,1.38294142126773));
#6024=CARTESIAN_POINT('Ctrl Pts',(1.09607155101171,8.6120789413123,1.67663290820799));
#6025=CARTESIAN_POINT('Ctrl Pts',(0.646819117253922,8.8204122746456,1.97032439514836));
#6026=CARTESIAN_POINT('Ctrl Pts',(0.110909353437527,9.02874560797896,2.00004246683495));
#6027=CARTESIAN_POINT('Ctrl Pts',(-0.425000410378858,9.23707894131227,2.02976053852165));
#6028=CARTESIAN_POINT('Ctrl Pts',(-0.903970915823293,9.44541227464561,1.78754226164552));
#6029=CARTESIAN_POINT('Ctrl Pts',(-1.38294142126773,9.65374560797894,1.5453239847695));
#6030=CARTESIAN_POINT('Ctrl Pts',(-1.67663290820805,9.86207894131228,1.09607155101171));
#6031=CARTESIAN_POINT('Ctrl Pts',(-1.97032439514836,10.0704122746456,0.64681911725392));
#6032=CARTESIAN_POINT('Ctrl Pts',(-2.00004246683499,10.278745607979,0.110909353437464));
#6033=CARTESIAN_POINT('Ctrl Pts',(-2.02976053852165,10.4870789413123,-0.425000410378862));
#6034=CARTESIAN_POINT('Ctrl Pts',(-1.78754226164558,10.6954122746456,-0.903970915823397));
#6035=CARTESIAN_POINT('Ctrl Pts',(-1.5453239847695,10.9037456079789,-1.38294142126775));
#6036=CARTESIAN_POINT('Ctrl Pts',(-1.09607155101171,11.1120789413123,-1.6766329082081));
#6037=CARTESIAN_POINT('Ctrl Pts',(-0.64681911725392,11.3204122746456,-1.97032439514837));
#6038=CARTESIAN_POINT('Ctrl Pts',(-0.11090935343753,11.528745607979,-2.00004246683503));
#6039=CARTESIAN_POINT('Ctrl Pts',(0.42500041037886,11.7370789413123,-2.02976053852167));
#6040=CARTESIAN_POINT('Ctrl Pts',(0.903970915823295,11.9454122746456,-1.78754226164558));
#6041=CARTESIAN_POINT('Ctrl Pts',(1.38294142126773,12.1537456079789,-1.54532398476955));
#6042=CARTESIAN_POINT('Ctrl Pts',(1.67663290820804,12.3620789413123,-1.09607155101172));
#6043=CARTESIAN_POINT('Ctrl Pts',(1.97032439514839,12.5704122746456,-0.646819117253935));
#6044=CARTESIAN_POINT('Ctrl Pts',(2.00004246683501,12.778745607979,-0.110909353437582));
#6045=CARTESIAN_POINT('Ctrl Pts',(2.02976053852165,12.9870789413123,0.425000410378862));
#6046=CARTESIAN_POINT('Ctrl Pts',(1.78754226164557,13.1954122746456,0.903970915823237));
#6047=CARTESIAN_POINT('Ctrl Pts',(1.5453239847695,13.4037456079789,1.38294142126772));
#6048=CARTESIAN_POINT('Ctrl Pts',(1.09607155101171,13.6120789413123,1.67663290820805));
#6049=CARTESIAN_POINT('Ctrl Pts',(0.646819117253922,13.8204122746456,1.97032439514837));
#6050=CARTESIAN_POINT('Ctrl Pts',(0.11090935343753,14.0287456079789,2.00004246683497));
#6051=CARTESIAN_POINT('Ctrl Pts',(-0.42500041037886,14.2370789413123,2.02976053852165));
#6052=CARTESIAN_POINT('Ctrl Pts',(-0.903970915823295,14.4454122746456,1.78754226164548));
#6053=CARTESIAN_POINT('Ctrl Pts',(-1.38294142126773,14.6537456079789,1.54532398476945));
#6054=CARTESIAN_POINT('Ctrl Pts',(-1.67663290820804,14.8620789413123,1.09607155101165));
#6055=CARTESIAN_POINT('Ctrl Pts',(-1.97032439514835,15.0704122746456,0.646819117253935));
#6056=CARTESIAN_POINT('Ctrl Pts',(-2.00004246683501,15.278745607979,0.110909353437471));
#6057=CARTESIAN_POINT('Ctrl Pts',(-2.02976053852165,15.4870789413123,-0.42500041037897));
#6058=CARTESIAN_POINT('Ctrl Pts',(-1.78754226164558,15.6954122746456,-0.903970915823307));
#6059=CARTESIAN_POINT('Ctrl Pts',(-1.5453239847695,15.9037456079789,-1.38294142126773));
#6060=CARTESIAN_POINT('Ctrl Pts',(-1.0960715510117,16.1120789413123,-1.67663290820808));
#6061=CARTESIAN_POINT('Ctrl Pts',(-0.64681911725392,16.3204122746456,-1.97032439514842));
#6062=CARTESIAN_POINT('Ctrl Pts',(-0.11090935343753,16.528745607979,-2.00004246683506));
#6063=CARTESIAN_POINT('Ctrl Pts',(0.425000410378862,16.7370789413123,-2.02976053852165));
#6064=CARTESIAN_POINT('Ctrl Pts',(0.903970915823309,16.9454122746456,-1.78754226164558));
#6065=CARTESIAN_POINT('Ctrl Pts',(1.38294142126773,17.1537456079789,-1.5453239847695));
#6066=CARTESIAN_POINT('Ctrl Pts',(1.67663290820804,17.3620789413123,-1.09607155101176));
#6067=CARTESIAN_POINT('Ctrl Pts',(1.97032439514836,17.5704122746456,-0.64681911725392));
#6068=CARTESIAN_POINT('Ctrl Pts',(2.00004246683501,17.778745607979,-0.110909353437541));
#6069=CARTESIAN_POINT('Ctrl Pts',(2.02976053852165,17.9870789413123,0.425000410378805));
#6070=CARTESIAN_POINT('Ctrl Pts',(1.78754226164558,18.1954122746456,0.903970915823279));
#6071=CARTESIAN_POINT('Ctrl Pts',(1.54532398476952,18.4037456079789,1.38294142126773));
#6072=CARTESIAN_POINT('Ctrl Pts',(1.09607155101171,18.6120789413123,1.67663290820799));
#6073=CARTESIAN_POINT('Ctrl Pts',(0.646819117253922,18.8204122746456,1.97032439514836));
#6074=CARTESIAN_POINT('Ctrl Pts',(0.110909353437529,19.028745607979,2.00004246683496));
#6075=CARTESIAN_POINT('Ctrl Pts',(-0.42500041037886,19.2370789413123,2.02976053852165));
#6076=CARTESIAN_POINT('Ctrl Pts',(-0.903970915823293,19.4454122746457,1.7875422616455));
#6077=CARTESIAN_POINT('Ctrl Pts',(-1.38294142126773,19.6537456079789,1.5453239847695));
#6078=CARTESIAN_POINT('Ctrl Pts',(-1.67663290820805,19.8620789413123,1.09607155101167));
#6079=CARTESIAN_POINT('Ctrl Pts',(-1.97032439514836,20.0704122746456,0.64681911725392));
#6080=CARTESIAN_POINT('Ctrl Pts',(-2.00004246683499,20.278745607979,0.110909353437444));
#6081=CARTESIAN_POINT('Ctrl Pts',(-2.02976053852164,20.4870789413123,-0.42500041037892));
#6082=CARTESIAN_POINT('Ctrl Pts',(-1.78754226164558,20.6954122746456,-0.903970915823355));
#6083=CARTESIAN_POINT('Ctrl Pts',(-1.54532398476949,20.903745607979,-1.38294142126777));
#6084=CARTESIAN_POINT('Ctrl Pts',(-1.09607155101172,21.1120789413123,-1.6766329082081));
#6085=CARTESIAN_POINT('Ctrl Pts',(-0.646819117253922,21.3204122746456,-1.97032439514837));
#6086=CARTESIAN_POINT('Ctrl Pts',(-0.11090935343753,21.528745607979,-2.00004246683501));
#6087=CARTESIAN_POINT('Ctrl Pts',(0.42500041037886,21.7370789413123,-2.02976053852164));
#6088=CARTESIAN_POINT('Ctrl Pts',(0.903970915823295,21.9454122746457,-1.78754226164561));
#6089=CARTESIAN_POINT('Ctrl Pts',(1.38294142126773,22.1537456079789,-1.54532398476955));
#6090=CARTESIAN_POINT('Ctrl Pts',(1.67663290820805,22.3620789413123,-1.09607155101173));
#6091=CARTESIAN_POINT('Ctrl Pts',(1.97032439514834,22.5704122746456,-0.64681911725392));
#6092=CARTESIAN_POINT('Ctrl Pts',(2.00004246683501,22.778745607979,-0.110909353437569));
#6093=CARTESIAN_POINT('Ctrl Pts',(2.02976053852168,22.9870789413123,0.425000410378862));
#6094=CARTESIAN_POINT('Ctrl Pts',(1.78754226164558,23.1954122746457,0.903970915823237));
#6095=CARTESIAN_POINT('Ctrl Pts',(1.5453239847695,23.4037456079789,1.38294142126772));
#6096=CARTESIAN_POINT('Ctrl Pts',(1.09607155101171,23.6120789413123,1.67663290820802));
#6097=CARTESIAN_POINT('Ctrl Pts',(0.646819117253936,23.8204122746456,1.97032439514837));
#6098=CARTESIAN_POINT('Ctrl Pts',(0.11090935343753,24.028745607979,2.00004246683493));
#6099=CARTESIAN_POINT('Ctrl Pts',(-0.42500041037886,24.2370789413123,2.02976053852166));
#6100=CARTESIAN_POINT('Ctrl Pts',(-0.903970915823295,24.4454122746457,1.78754226164548));
#6101=CARTESIAN_POINT('Ctrl Pts',(-1.38294142126772,24.653745607979,1.54532398476942));
#6102=CARTESIAN_POINT('Ctrl Pts',(-1.67663290820803,24.8620789413123,1.09607155101166));
#6103=CARTESIAN_POINT('Ctrl Pts',(-1.97032439514836,25.0704122746456,0.646819117253935));
#6104=CARTESIAN_POINT('Ctrl Pts',(-2.00004246683501,25.278745607979,0.110909353437478));
#6105=CARTESIAN_POINT('Ctrl Pts',(-2.02976053852165,25.4870789413123,-0.425000410378891));
#6106=CARTESIAN_POINT('Ctrl Pts',(-1.78754226164558,25.6954122746456,-0.903970915823307));
#6107=CARTESIAN_POINT('Ctrl Pts',(-1.5453239847695,25.903745607979,-1.38294142126773));
#6108=CARTESIAN_POINT('Ctrl Pts',(-1.09607155101171,26.1120789413123,-1.67663290820807));
#6109=CARTESIAN_POINT('Ctrl Pts',(-0.64681911725392,26.3204122746456,-1.97032439514842));
#6110=CARTESIAN_POINT('Ctrl Pts',(-0.11090935343753,26.528745607979,-2.00004246683504));
#6111=CARTESIAN_POINT('Ctrl Pts',(0.425000410378875,26.7370789413123,-2.02976053852165));
#6112=CARTESIAN_POINT('Ctrl Pts',(0.903970915823309,26.9454122746457,-1.78754226164563));
#6113=CARTESIAN_POINT('Ctrl Pts',(1.38294142126773,27.1537456079789,-1.5453239847695));
#6114=CARTESIAN_POINT('Ctrl Pts',(1.67663290820802,27.3620789413123,-1.09607155101175));
#6115=CARTESIAN_POINT('Ctrl Pts',(1.97032439514836,27.5704122746456,-0.646819117253949));
#6116=CARTESIAN_POINT('Ctrl Pts',(2.00004246683498,27.778745607979,-0.110909353437534));
#6117=CARTESIAN_POINT('Ctrl Pts',(2.02976053852165,27.9870789413123,0.425000410378855));
#6118=CARTESIAN_POINT('Ctrl Pts',(1.78754226164558,28.1954122746457,0.903970915823265));
#6119=CARTESIAN_POINT('Ctrl Pts',(1.54532398476949,28.403745607979,1.38294142126772));
#6120=CARTESIAN_POINT('Ctrl Pts',(1.09607155101171,28.6120789413123,1.676632908208));
#6121=CARTESIAN_POINT('Ctrl Pts',(0.646819117253922,28.8204122746456,1.97032439514833));
#6122=CARTESIAN_POINT('Ctrl Pts',(0.110909353437544,29.028745607979,2.00004246683497));
#6123=CARTESIAN_POINT('Ctrl Pts',(-0.42500041037886,29.2370789413123,2.02976053852165));
#6124=CARTESIAN_POINT('Ctrl Pts',(-0.903970915823293,29.4454122746457,1.78754226164552));
#6125=CARTESIAN_POINT('Ctrl Pts',(-1.38294142126773,29.653745607979,1.54532398476947));
#6126=CARTESIAN_POINT('Ctrl Pts',(-1.67663290820805,29.8620789413123,1.09607155101164));
#6127=CARTESIAN_POINT('Ctrl Pts',(-1.97032439514836,30.0704122746456,0.646819117253891));
#6128=CARTESIAN_POINT('Ctrl Pts',(-2.00004246683501,30.278745607979,0.110909353437458));
#6129=CARTESIAN_POINT('Ctrl Pts',(-2.02976053852165,30.4870789413123,-0.42500041037892));
#6130=CARTESIAN_POINT('Ctrl Pts',(-1.78754226164556,30.6954122746457,-0.903970915823342));
#6131=CARTESIAN_POINT('Ctrl Pts',(-1.5453239847695,30.903745607979,-1.3829414212677));
#6132=CARTESIAN_POINT('Ctrl Pts',(-1.09607155101171,31.1120789413123,-1.6766329082081));
#6133=CARTESIAN_POINT('Ctrl Pts',(-0.64681911725392,31.3204122746456,-1.97032439514837));
#6134=CARTESIAN_POINT('Ctrl Pts',(-0.110909353437529,31.528745607979,-2.00004246683501));
#6135=CARTESIAN_POINT('Ctrl Pts',(0.425000410378862,31.7370789413123,-2.02976053852167));
#6136=CARTESIAN_POINT('Ctrl Pts',(0.903970915823283,31.9454122746457,-1.7875422616456));
#6137=CARTESIAN_POINT('Ctrl Pts',(1.38294142126773,32.153745607979,-1.54532398476955));
#6138=CARTESIAN_POINT('Ctrl Pts',(1.67663290820804,32.3620789413124,-1.09607155101176));
#6139=CARTESIAN_POINT('Ctrl Pts',(1.97032439514836,32.5704122746456,-0.64681911725392));
#6140=CARTESIAN_POINT('Ctrl Pts',(2.00004246683501,32.778745607979,-0.110909353437541));
#6141=CARTESIAN_POINT('Ctrl Pts',(2.02976053852165,32.9870789413124,0.425000410378833));
#6142=CARTESIAN_POINT('Ctrl Pts',(1.78754226164557,33.1954122746457,0.903970915823237));
#6143=CARTESIAN_POINT('Ctrl Pts',(1.5453239847695,33.4037456079789,1.38294142126775));
#6144=CARTESIAN_POINT('Ctrl Pts',(1.09607155101171,33.6120789413123,1.67663290820803));
#6145=CARTESIAN_POINT('Ctrl Pts',(0.646819117253922,33.8204122746456,1.97032439514837));
#6146=CARTESIAN_POINT('Ctrl Pts',(0.11090935343753,34.028745607979,2.00004246683493));
#6147=CARTESIAN_POINT('Ctrl Pts',(-0.42500041037886,34.2370789413123,2.02976053852164));
#6148=CARTESIAN_POINT('Ctrl Pts',(-0.903970915823295,34.4454122746457,1.78754226164551));
#6149=CARTESIAN_POINT('Ctrl Pts',(-1.38294142126774,34.653745607979,1.54532398476948));
#6150=CARTESIAN_POINT('Ctrl Pts',(-1.67663290820803,34.8620789413123,1.09607155101167));
#6151=CARTESIAN_POINT('Ctrl Pts',(-1.97032439514836,35.0704122746456,0.646819117253935));
#6152=CARTESIAN_POINT('Ctrl Pts',(-2.00004246683501,35.2787456079791,0.110909353437478));
#6153=CARTESIAN_POINT('Ctrl Pts',(-2.02976053852165,35.4870789413123,-0.425000410378905));
#6154=CARTESIAN_POINT('Ctrl Pts',(-1.78754226164558,35.6954122746457,-0.903970915823328));
#6155=CARTESIAN_POINT('Ctrl Pts',(-1.5453239847695,35.903745607979,-1.38294142126775));
#6156=CARTESIAN_POINT('Ctrl Pts',(-1.09607155101171,36.1120789413124,-1.67663290820807));
#6157=CARTESIAN_POINT('Ctrl Pts',(-0.646819117253907,36.3204122746457,-1.97032439514837));
#6158=CARTESIAN_POINT('Ctrl Pts',(-0.11090935343753,36.528745607979,-2.00004246683505));
#6159=CARTESIAN_POINT('Ctrl Pts',(0.42500041037886,36.7370789413123,-2.02976053852166));
#6160=CARTESIAN_POINT('Ctrl Pts',(0.903970915823295,36.9454122746457,-1.78754226164563));
#6161=CARTESIAN_POINT('Ctrl Pts',(1.38294142126773,37.1537456079789,-1.5453239847695));
#6162=CARTESIAN_POINT('Ctrl Pts',(1.67663290820805,37.3620789413124,-1.09607155101176));
#6163=CARTESIAN_POINT('Ctrl Pts',(1.97032439514836,37.5704122746456,-0.64681911725392));
#6164=CARTESIAN_POINT('Ctrl Pts',(2.00004246683501,37.778745607979,-0.110909353437575));
#6165=CARTESIAN_POINT('Ctrl Pts',(2.02976053852168,37.9870789413124,0.425000410378855));
#6166=CARTESIAN_POINT('Ctrl Pts',(1.78754226164558,38.1954122746457,0.903970915823252));
#6167=CARTESIAN_POINT('Ctrl Pts',(1.5453239847695,38.4037456079789,1.38294142126773));
#6168=CARTESIAN_POINT('Ctrl Pts',(1.09607155101173,38.6120789413124,1.676632908208));
#6169=CARTESIAN_POINT('Ctrl Pts',(0.646819117253922,38.8204122746457,1.97032439514837));
#6170=CARTESIAN_POINT('Ctrl Pts',(0.110909353437544,39.028745607979,2.00004246683497));
#6171=CARTESIAN_POINT('Ctrl Pts',(-0.425000410378846,39.2370789413124,2.02976053852167));
#6172=CARTESIAN_POINT('Ctrl Pts',(-0.903970915823281,39.4454122746457,1.78754226164553));
#6173=CARTESIAN_POINT('Ctrl Pts',(-1.38294142126773,39.653745607979,1.54532398476946));
#6174=CARTESIAN_POINT('Ctrl Pts',(-1.67663290820805,39.8620789413124,1.09607155101165));
#6175=CARTESIAN_POINT('Ctrl Pts',(-1.97032439514836,40.0704122746457,0.646819117253935));
#6176=CARTESIAN_POINT('Ctrl Pts',(-2.00004246683501,40.278745607979,0.110909353437458));
#6177=CARTESIAN_POINT('Ctrl Pts',(-2.00002123304185,0.278745610073468,0.110909354270813));
#6178=CARTESIAN_POINT('Ctrl Pts',(-2.0297393049518,0.487078943406699,-0.42499471996778));
#6179=CARTESIAN_POINT('Ctrl Pts',(-1.78752387305798,0.695412276740089,-0.903960298205047));
#6180=CARTESIAN_POINT('Ctrl Pts',(-1.54530844116415,0.903745610073333,-1.38292587644223));
#6181=CARTESIAN_POINT('Ctrl Pts',(-1.09606093483686,1.11207894340676,-1.67661451878712));
#6182=CARTESIAN_POINT('Ctrl Pts',(-0.646813428509569,1.32041227674011,-1.97030316113191));
#6183=CARTESIAN_POINT('Ctrl Pts',(-0.110909354270893,1.52874561007344,-2.00002123304186));
#6184=CARTESIAN_POINT('Ctrl Pts',(0.424994719967758,1.7370789434067,-2.02973930495184));
#6185=CARTESIAN_POINT('Ctrl Pts',(0.903960298204994,1.94541227674011,-1.78752387305798));
#6186=CARTESIAN_POINT('Ctrl Pts',(1.38292587644223,2.15374561007344,-1.54530844116415));
#6187=CARTESIAN_POINT('Ctrl Pts',(1.67661451878707,2.36207894340677,-1.09606093483686));
#6188=CARTESIAN_POINT('Ctrl Pts',(1.97030316113191,2.57041227674009,-0.646813428509584));
#6189=CARTESIAN_POINT('Ctrl Pts',(2.00002123304188,2.77874561007344,-0.110909354270911));
#6190=CARTESIAN_POINT('Ctrl Pts',(2.0297393049518,2.98707894340676,0.424994719967736));
#6191=CARTESIAN_POINT('Ctrl Pts',(1.78752387305798,3.1954122767401,0.903960298204943));
#6192=CARTESIAN_POINT('Ctrl Pts',(1.54530844116415,3.40374561007338,1.38292587644222));
#6193=CARTESIAN_POINT('Ctrl Pts',(1.09606093483686,3.61207894340677,1.67661451878706));
#6194=CARTESIAN_POINT('Ctrl Pts',(0.646813428509572,3.82041227674006,1.97030316113189));
#6195=CARTESIAN_POINT('Ctrl Pts',(0.110909354270907,4.02874561007344,2.0000212330418));
#6196=CARTESIAN_POINT('Ctrl Pts',(-0.424994719967742,4.23707894340673,2.02973930495178));
#6197=CARTESIAN_POINT('Ctrl Pts',(-0.903960298204994,4.44541227674011,1.78752387305797));
#6198=CARTESIAN_POINT('Ctrl Pts',(-1.38292587644223,4.65374561007344,1.5453084411641));
#6199=CARTESIAN_POINT('Ctrl Pts',(-1.67661451878708,4.8620789434068,1.0960609348368));
#6200=CARTESIAN_POINT('Ctrl Pts',(-1.9703031611319,5.07041227674005,0.646813428509555));
#6201=CARTESIAN_POINT('Ctrl Pts',(-2.00002123304185,5.27874561007342,0.110909354270813));
#6202=CARTESIAN_POINT('Ctrl Pts',(-2.0297393049518,5.48707894340671,-0.424994719967823));
#6203=CARTESIAN_POINT('Ctrl Pts',(-1.78752387305798,5.6954122767401,-0.903960298205047));
#6204=CARTESIAN_POINT('Ctrl Pts',(-1.54530844116415,5.90374561007338,-1.38292587644222));
#6205=CARTESIAN_POINT('Ctrl Pts',(-1.09606093483685,6.11207894340678,-1.67661451878707));
#6206=CARTESIAN_POINT('Ctrl Pts',(-0.646813428509557,6.3204122767401,-1.97030316113191));
#6207=CARTESIAN_POINT('Ctrl Pts',(-0.110909354270905,6.52874561007347,-2.00002123304191));
#6208=CARTESIAN_POINT('Ctrl Pts',(0.424994719967756,6.73707894340672,-2.02973930495181));
#6209=CARTESIAN_POINT('Ctrl Pts',(0.903960298204995,6.94541227674014,-1.78752387305798));
#6210=CARTESIAN_POINT('Ctrl Pts',(1.38292587644225,7.15374561007342,-1.54530844116421));
#6211=CARTESIAN_POINT('Ctrl Pts',(1.67661451878704,7.36207894340677,-1.09606093483692));
#6212=CARTESIAN_POINT('Ctrl Pts',(1.97030316113191,7.57041227674011,-0.646813428509569));
#6213=CARTESIAN_POINT('Ctrl Pts',(2.00002123304185,7.77874561007349,-0.110909354270917));
#6214=CARTESIAN_POINT('Ctrl Pts',(2.0297393049518,7.98707894340672,0.424994719967736));
#6215=CARTESIAN_POINT('Ctrl Pts',(1.78752387305798,8.19541227674012,0.903960298204985));
#6216=CARTESIAN_POINT('Ctrl Pts',(1.54530844116417,8.40374561007341,1.38292587644223));
#6217=CARTESIAN_POINT('Ctrl Pts',(1.09606093483686,8.6120789434068,1.67661451878701));
#6218=CARTESIAN_POINT('Ctrl Pts',(0.646813428509572,8.82041227674011,1.9703031611319));
#6219=CARTESIAN_POINT('Ctrl Pts',(0.110909354270904,9.02874561007346,2.00002123304179));
#6220=CARTESIAN_POINT('Ctrl Pts',(-0.424994719967754,9.23707894340678,2.0297393049518));
#6221=CARTESIAN_POINT('Ctrl Pts',(-0.903960298204992,9.44541227674011,1.78752387305792));
#6222=CARTESIAN_POINT('Ctrl Pts',(-1.38292587644223,9.65374561007344,1.54530844116415));
#6223=CARTESIAN_POINT('Ctrl Pts',(-1.67661451878707,9.86207894340678,1.09606093483686));
#6224=CARTESIAN_POINT('Ctrl Pts',(-1.97030316113191,10.0704122767401,0.646813428509569));
#6225=CARTESIAN_POINT('Ctrl Pts',(-2.00002123304184,10.2787456100735,0.110909354270841));
#6226=CARTESIAN_POINT('Ctrl Pts',(-2.0297393049518,10.4870789434068,-0.424994719967758));
#6227=CARTESIAN_POINT('Ctrl Pts',(-1.78752387305798,10.6954122767401,-0.903960298205096));
#6228=CARTESIAN_POINT('Ctrl Pts',(-1.54530844116415,10.9037456100734,-1.38292587644225));
#6229=CARTESIAN_POINT('Ctrl Pts',(-1.09606093483686,11.1120789434068,-1.67661451878712));
#6230=CARTESIAN_POINT('Ctrl Pts',(-0.646813428509569,11.3204122767401,-1.97030316113191));
#6231=CARTESIAN_POINT('Ctrl Pts',(-0.110909354270907,11.5287456100735,-2.00002123304188));
#6232=CARTESIAN_POINT('Ctrl Pts',(0.424994719967756,11.7370789434068,-2.02973930495182));
#6233=CARTESIAN_POINT('Ctrl Pts',(0.903960298204994,11.9454122767401,-1.78752387305798));
#6234=CARTESIAN_POINT('Ctrl Pts',(1.38292587644223,12.1537456100734,-1.5453084411642));
#6235=CARTESIAN_POINT('Ctrl Pts',(1.67661451878707,12.3620789434068,-1.09606093483686));
#6236=CARTESIAN_POINT('Ctrl Pts',(1.97030316113194,12.5704122767401,-0.646813428509584));
#6237=CARTESIAN_POINT('Ctrl Pts',(2.00002123304185,12.7787456100735,-0.110909354270959));
#6238=CARTESIAN_POINT('Ctrl Pts',(2.0297393049518,12.9870789434068,0.424994719967758));
#6239=CARTESIAN_POINT('Ctrl Pts',(1.78752387305797,13.1954122767401,0.903960298204936));
#6240=CARTESIAN_POINT('Ctrl Pts',(1.54530844116415,13.4037456100734,1.38292587644223));
#6241=CARTESIAN_POINT('Ctrl Pts',(1.09606093483686,13.6120789434068,1.67661451878707));
#6242=CARTESIAN_POINT('Ctrl Pts',(0.646813428509572,13.8204122767401,1.97030316113191));
#6243=CARTESIAN_POINT('Ctrl Pts',(0.110909354270907,14.0287456100735,2.00002123304182));
#6244=CARTESIAN_POINT('Ctrl Pts',(-0.424994719967756,14.2370789434068,2.0297393049518));
#6245=CARTESIAN_POINT('Ctrl Pts',(-0.903960298204994,14.4454122767402,1.78752387305788));
#6246=CARTESIAN_POINT('Ctrl Pts',(-1.38292587644223,14.6537456100734,1.5453084411641));
#6247=CARTESIAN_POINT('Ctrl Pts',(-1.67661451878707,14.8620789434068,1.0960609348368));
#6248=CARTESIAN_POINT('Ctrl Pts',(-1.97030316113189,15.0704122767401,0.646813428509584));
#6249=CARTESIAN_POINT('Ctrl Pts',(-2.00002123304185,15.2787456100735,0.110909354270848));
#6250=CARTESIAN_POINT('Ctrl Pts',(-2.0297393049518,15.4870789434068,-0.424994719967866));
#6251=CARTESIAN_POINT('Ctrl Pts',(-1.78752387305798,15.6954122767401,-0.903960298205006));
#6252=CARTESIAN_POINT('Ctrl Pts',(-1.54530844116415,15.9037456100734,-1.38292587644223));
#6253=CARTESIAN_POINT('Ctrl Pts',(-1.09606093483685,16.1120789434068,-1.6766145187871));
#6254=CARTESIAN_POINT('Ctrl Pts',(-0.646813428509569,16.3204122767401,-1.97030316113196));
#6255=CARTESIAN_POINT('Ctrl Pts',(-0.110909354270907,16.5287456100735,-2.0000212330419));
#6256=CARTESIAN_POINT('Ctrl Pts',(0.424994719967758,16.7370789434068,-2.0297393049518));
#6257=CARTESIAN_POINT('Ctrl Pts',(0.903960298205007,16.9454122767401,-1.78752387305798));
#6258=CARTESIAN_POINT('Ctrl Pts',(1.38292587644223,17.1537456100734,-1.54530844116415));
#6259=CARTESIAN_POINT('Ctrl Pts',(1.67661451878707,17.3620789434068,-1.09606093483691));
#6260=CARTESIAN_POINT('Ctrl Pts',(1.97030316113191,17.5704122767401,-0.646813428509569));
#6261=CARTESIAN_POINT('Ctrl Pts',(2.00002123304185,17.7787456100735,-0.110909354270917));
#6262=CARTESIAN_POINT('Ctrl Pts',(2.0297393049518,17.9870789434068,0.424994719967701));
#6263=CARTESIAN_POINT('Ctrl Pts',(1.78752387305798,18.1954122767401,0.903960298204978));
#6264=CARTESIAN_POINT('Ctrl Pts',(1.54530844116417,18.4037456100734,1.38292587644223));
#6265=CARTESIAN_POINT('Ctrl Pts',(1.09606093483686,18.6120789434068,1.67661451878701));
#6266=CARTESIAN_POINT('Ctrl Pts',(0.646813428509572,18.8204122767401,1.9703031611319));
#6267=CARTESIAN_POINT('Ctrl Pts',(0.110909354270905,19.0287456100735,2.00002123304181));
#6268=CARTESIAN_POINT('Ctrl Pts',(-0.424994719967756,19.2370789434068,2.0297393049518));
#6269=CARTESIAN_POINT('Ctrl Pts',(-0.903960298204992,19.4454122767402,1.7875238730579));
#6270=CARTESIAN_POINT('Ctrl Pts',(-1.38292587644223,19.6537456100734,1.54530844116415));
#6271=CARTESIAN_POINT('Ctrl Pts',(-1.67661451878707,19.8620789434068,1.09606093483682));
#6272=CARTESIAN_POINT('Ctrl Pts',(-1.97030316113191,20.0704122767401,0.646813428509569));
#6273=CARTESIAN_POINT('Ctrl Pts',(-2.00002123304184,20.2787456100735,0.11090935427082));
#6274=CARTESIAN_POINT('Ctrl Pts',(-2.02973930495179,20.4870789434068,-0.424994719967816));
#6275=CARTESIAN_POINT('Ctrl Pts',(-1.78752387305798,20.6954122767402,-0.903960298205054));
#6276=CARTESIAN_POINT('Ctrl Pts',(-1.54530844116414,20.9037456100735,-1.38292587644227));
#6277=CARTESIAN_POINT('Ctrl Pts',(-1.09606093483687,21.1120789434068,-1.67661451878712));
#6278=CARTESIAN_POINT('Ctrl Pts',(-0.646813428509572,21.3204122767401,-1.97030316113191));
#6279=CARTESIAN_POINT('Ctrl Pts',(-0.110909354270907,21.5287456100735,-2.00002123304186));
#6280=CARTESIAN_POINT('Ctrl Pts',(0.424994719967756,21.7370789434068,-2.0297393049518));
#6281=CARTESIAN_POINT('Ctrl Pts',(0.903960298204994,21.9454122767402,-1.78752387305801));
#6282=CARTESIAN_POINT('Ctrl Pts',(1.38292587644223,22.1537456100734,-1.5453084411642));
#6283=CARTESIAN_POINT('Ctrl Pts',(1.67661451878707,22.3620789434069,-1.09606093483688));
#6284=CARTESIAN_POINT('Ctrl Pts',(1.97030316113188,22.5704122767401,-0.646813428509569));
#6285=CARTESIAN_POINT('Ctrl Pts',(2.00002123304185,22.7787456100735,-0.110909354270945));
#6286=CARTESIAN_POINT('Ctrl Pts',(2.02973930495183,22.9870789434068,0.424994719967758));
#6287=CARTESIAN_POINT('Ctrl Pts',(1.78752387305798,23.1954122767402,0.903960298204936));
#6288=CARTESIAN_POINT('Ctrl Pts',(1.54530844116415,23.4037456100734,1.38292587644223));
#6289=CARTESIAN_POINT('Ctrl Pts',(1.09606093483686,23.6120789434068,1.67661451878704));
#6290=CARTESIAN_POINT('Ctrl Pts',(0.646813428509586,23.8204122767401,1.97030316113191));
#6291=CARTESIAN_POINT('Ctrl Pts',(0.110909354270907,24.0287456100735,2.00002123304177));
#6292=CARTESIAN_POINT('Ctrl Pts',(-0.424994719967756,24.2370789434068,2.02973930495181));
#6293=CARTESIAN_POINT('Ctrl Pts',(-0.903960298204994,24.4454122767402,1.78752387305788));
#6294=CARTESIAN_POINT('Ctrl Pts',(-1.38292587644222,24.6537456100735,1.54530844116407));
#6295=CARTESIAN_POINT('Ctrl Pts',(-1.67661451878706,24.8620789434068,1.09606093483681));
#6296=CARTESIAN_POINT('Ctrl Pts',(-1.97030316113191,25.0704122767401,0.646813428509584));
#6297=CARTESIAN_POINT('Ctrl Pts',(-2.00002123304185,25.2787456100735,0.110909354270855));
#6298=CARTESIAN_POINT('Ctrl Pts',(-2.0297393049518,25.4870789434068,-0.424994719967787));
#6299=CARTESIAN_POINT('Ctrl Pts',(-1.78752387305798,25.6954122767401,-0.903960298205006));
#6300=CARTESIAN_POINT('Ctrl Pts',(-1.54530844116415,25.9037456100735,-1.38292587644223));
#6301=CARTESIAN_POINT('Ctrl Pts',(-1.09606093483686,26.1120789434068,-1.6766145187871));
#6302=CARTESIAN_POINT('Ctrl Pts',(-0.646813428509569,26.3204122767401,-1.97030316113196));
#6303=CARTESIAN_POINT('Ctrl Pts',(-0.110909354270907,26.5287456100735,-2.00002123304189));
#6304=CARTESIAN_POINT('Ctrl Pts',(0.424994719967771,26.7370789434068,-2.0297393049518));
#6305=CARTESIAN_POINT('Ctrl Pts',(0.903960298205007,26.9454122767402,-1.78752387305803));
#6306=CARTESIAN_POINT('Ctrl Pts',(1.38292587644223,27.1537456100734,-1.54530844116415));
#6307=CARTESIAN_POINT('Ctrl Pts',(1.67661451878704,27.3620789434068,-1.0960609348369));
#6308=CARTESIAN_POINT('Ctrl Pts',(1.97030316113191,27.5704122767401,-0.646813428509598));
#6309=CARTESIAN_POINT('Ctrl Pts',(2.00002123304183,27.7787456100735,-0.110909354270911));
#6310=CARTESIAN_POINT('Ctrl Pts',(2.0297393049518,27.9870789434068,0.424994719967751));
#6311=CARTESIAN_POINT('Ctrl Pts',(1.78752387305798,28.1954122767402,0.903960298204964));
#6312=CARTESIAN_POINT('Ctrl Pts',(1.54530844116414,28.4037456100735,1.38292587644223));
#6313=CARTESIAN_POINT('Ctrl Pts',(1.09606093483686,28.6120789434068,1.67661451878702));
#6314=CARTESIAN_POINT('Ctrl Pts',(0.646813428509572,28.8204122767401,1.97030316113188));
#6315=CARTESIAN_POINT('Ctrl Pts',(0.110909354270921,29.0287456100735,2.00002123304182));
#6316=CARTESIAN_POINT('Ctrl Pts',(-0.424994719967756,29.2370789434068,2.0297393049518));
#6317=CARTESIAN_POINT('Ctrl Pts',(-0.903960298204992,29.4454122767402,1.78752387305792));
#6318=CARTESIAN_POINT('Ctrl Pts',(-1.38292587644223,29.6537456100735,1.54530844116412));
#6319=CARTESIAN_POINT('Ctrl Pts',(-1.67661451878707,29.8620789434068,1.09606093483679));
#6320=CARTESIAN_POINT('Ctrl Pts',(-1.97030316113191,30.0704122767401,0.646813428509541));
#6321=CARTESIAN_POINT('Ctrl Pts',(-2.00002123304185,30.2787456100735,0.110909354270834));
#6322=CARTESIAN_POINT('Ctrl Pts',(-2.0297393049518,30.4870789434068,-0.424994719967816));
#6323=CARTESIAN_POINT('Ctrl Pts',(-1.78752387305796,30.6954122767402,-0.90396029820504));
#6324=CARTESIAN_POINT('Ctrl Pts',(-1.54530844116415,30.9037456100735,-1.3829258764422));
#6325=CARTESIAN_POINT('Ctrl Pts',(-1.09606093483686,31.1120789434068,-1.67661451878712));
#6326=CARTESIAN_POINT('Ctrl Pts',(-0.646813428509569,31.3204122767401,-1.97030316113191));
#6327=CARTESIAN_POINT('Ctrl Pts',(-0.110909354270905,31.5287456100735,-2.00002123304186));
#6328=CARTESIAN_POINT('Ctrl Pts',(0.424994719967758,31.7370789434068,-2.02973930495182));
#6329=CARTESIAN_POINT('Ctrl Pts',(0.903960298204981,31.9454122767402,-1.787523873058));
#6330=CARTESIAN_POINT('Ctrl Pts',(1.38292587644223,32.1537456100735,-1.5453084411642));
#6331=CARTESIAN_POINT('Ctrl Pts',(1.67661451878707,32.3620789434069,-1.09606093483691));
#6332=CARTESIAN_POINT('Ctrl Pts',(1.97030316113191,32.5704122767401,-0.646813428509569));
#6333=CARTESIAN_POINT('Ctrl Pts',(2.00002123304185,32.7787456100735,-0.110909354270917));
#6334=CARTESIAN_POINT('Ctrl Pts',(2.0297393049518,32.9870789434069,0.424994719967729));
#6335=CARTESIAN_POINT('Ctrl Pts',(1.78752387305797,33.1954122767402,0.903960298204936));
#6336=CARTESIAN_POINT('Ctrl Pts',(1.54530844116415,33.4037456100734,1.38292587644225));
#6337=CARTESIAN_POINT('Ctrl Pts',(1.09606093483686,33.6120789434068,1.67661451878706));
#6338=CARTESIAN_POINT('Ctrl Pts',(0.646813428509572,33.8204122767401,1.97030316113191));
#6339=CARTESIAN_POINT('Ctrl Pts',(0.110909354270907,34.0287456100735,2.00002123304178));
#6340=CARTESIAN_POINT('Ctrl Pts',(-0.424994719967756,34.2370789434068,2.0297393049518));
#6341=CARTESIAN_POINT('Ctrl Pts',(-0.903960298204994,34.4454122767402,1.78752387305791));
#6342=CARTESIAN_POINT('Ctrl Pts',(-1.38292587644225,34.6537456100735,1.54530844116413));
#6343=CARTESIAN_POINT('Ctrl Pts',(-1.67661451878706,34.8620789434068,1.09606093483682));
#6344=CARTESIAN_POINT('Ctrl Pts',(-1.9703031611319,35.0704122767402,0.646813428509584));
#6345=CARTESIAN_POINT('Ctrl Pts',(-2.00002123304185,35.2787456100736,0.110909354270855));
#6346=CARTESIAN_POINT('Ctrl Pts',(-2.0297393049518,35.4870789434068,-0.424994719967801));
#6347=CARTESIAN_POINT('Ctrl Pts',(-1.78752387305798,35.6954122767402,-0.903960298205026));
#6348=CARTESIAN_POINT('Ctrl Pts',(-1.54530844116415,35.9037456100735,-1.38292587644225));
#6349=CARTESIAN_POINT('Ctrl Pts',(-1.09606093483686,36.1120789434069,-1.67661451878709));
#6350=CARTESIAN_POINT('Ctrl Pts',(-0.646813428509557,36.3204122767402,-1.97030316113191));
#6351=CARTESIAN_POINT('Ctrl Pts',(-0.110909354270907,36.5287456100735,-2.0000212330419));
#6352=CARTESIAN_POINT('Ctrl Pts',(0.424994719967756,36.7370789434068,-2.02973930495181));
#6353=CARTESIAN_POINT('Ctrl Pts',(0.903960298204994,36.9454122767402,-1.78752387305804));
#6354=CARTESIAN_POINT('Ctrl Pts',(1.38292587644223,37.1537456100734,-1.54530844116415));
#6355=CARTESIAN_POINT('Ctrl Pts',(1.67661451878707,37.3620789434069,-1.09606093483691));
#6356=CARTESIAN_POINT('Ctrl Pts',(1.97030316113191,37.5704122767401,-0.646813428509569));
#6357=CARTESIAN_POINT('Ctrl Pts',(2.00002123304185,37.7787456100735,-0.110909354270952));
#6358=CARTESIAN_POINT('Ctrl Pts',(2.02973930495183,37.9870789434069,0.424994719967751));
#6359=CARTESIAN_POINT('Ctrl Pts',(1.78752387305798,38.1954122767402,0.90396029820495));
#6360=CARTESIAN_POINT('Ctrl Pts',(1.54530844116415,38.4037456100734,1.38292587644223));
#6361=CARTESIAN_POINT('Ctrl Pts',(1.09606093483688,38.6120789434069,1.67661451878703));
#6362=CARTESIAN_POINT('Ctrl Pts',(0.646813428509572,38.8204122767402,1.97030316113192));
#6363=CARTESIAN_POINT('Ctrl Pts',(0.110909354270921,39.0287456100735,2.00002123304182));
#6364=CARTESIAN_POINT('Ctrl Pts',(-0.424994719967742,39.2370789434069,2.02973930495182));
#6365=CARTESIAN_POINT('Ctrl Pts',(-0.90396029820498,39.4454122767402,1.78752387305793));
#6366=CARTESIAN_POINT('Ctrl Pts',(-1.38292587644223,39.6537456100735,1.54530844116411));
#6367=CARTESIAN_POINT('Ctrl Pts',(-1.67661451878707,39.8620789434069,1.0960609348368));
#6368=CARTESIAN_POINT('Ctrl Pts',(-1.97030316113191,40.0704122767402,0.646813428509584));
#6369=CARTESIAN_POINT('Ctrl Pts',(-2.00002123304185,40.2787456100735,0.110909354270834));
#6370=CARTESIAN_POINT('Ctrl Pts',(-2.,0.278745610073468,0.110909354270813));
#6371=CARTESIAN_POINT('Ctrl Pts',(-2.02971807190995,0.487078943406699,-0.424989030591362));
#6372=CARTESIAN_POINT('Ctrl Pts',(-1.78750548470433,0.695412276740089,-0.90394968168412));
#6373=CARTESIAN_POINT('Ctrl Pts',(-1.54529289749872,0.903745610073333,-1.3829103327768));
#6374=CARTESIAN_POINT('Ctrl Pts',(-1.09605031831593,1.11207894340676,-1.67659613043348));
#6375=CARTESIAN_POINT('Ctrl Pts',(-0.646807739133152,1.32041227674011,-1.97028192809006));
#6376=CARTESIAN_POINT('Ctrl Pts',(-0.110909354270893,1.52874561007344,-2.00000000000001));
#6377=CARTESIAN_POINT('Ctrl Pts',(0.42498903059134,1.7370789434067,-2.02971807190998));
#6378=CARTESIAN_POINT('Ctrl Pts',(0.903949681684066,1.94541227674011,-1.78750548470433));
#6379=CARTESIAN_POINT('Ctrl Pts',(1.38291033277679,2.15374561007344,-1.54529289749872));
#6380=CARTESIAN_POINT('Ctrl Pts',(1.67659613043343,2.36207894340677,-1.09605031831594));
#6381=CARTESIAN_POINT('Ctrl Pts',(1.97028192809005,2.57041227674009,-0.646807739133166));
#6382=CARTESIAN_POINT('Ctrl Pts',(2.00000000000003,2.77874561007344,-0.110909354270911));
#6383=CARTESIAN_POINT('Ctrl Pts',(2.02971807190995,2.98707894340676,0.424989030591319));
#6384=CARTESIAN_POINT('Ctrl Pts',(1.78750548470433,3.1954122767401,0.903949681684016));
#6385=CARTESIAN_POINT('Ctrl Pts',(1.54529289749872,3.40374561007338,1.38291033277678));
#6386=CARTESIAN_POINT('Ctrl Pts',(1.09605031831593,3.61207894340677,1.67659613043342));
#6387=CARTESIAN_POINT('Ctrl Pts',(0.646807739133154,3.82041227674006,1.97028192809004));
#6388=CARTESIAN_POINT('Ctrl Pts',(0.110909354270907,4.02874561007344,1.99999999999995));
#6389=CARTESIAN_POINT('Ctrl Pts',(-0.424989030591324,4.23707894340672,2.02971807190993));
#6390=CARTESIAN_POINT('Ctrl Pts',(-0.903949681684066,4.44541227674011,1.78750548470433));
#6391=CARTESIAN_POINT('Ctrl Pts',(-1.38291033277679,4.65374561007344,1.54529289749866));
#6392=CARTESIAN_POINT('Ctrl Pts',(-1.67659613043344,4.8620789434068,1.09605031831587));
#6393=CARTESIAN_POINT('Ctrl Pts',(-1.97028192809005,5.07041227674005,0.646807739133138));
#6394=CARTESIAN_POINT('Ctrl Pts',(-2.,5.27874561007342,0.110909354270813));
#6395=CARTESIAN_POINT('Ctrl Pts',(-2.02971807190995,5.48707894340671,-0.424989030591405));
#6396=CARTESIAN_POINT('Ctrl Pts',(-1.78750548470433,5.6954122767401,-0.90394968168412));
#6397=CARTESIAN_POINT('Ctrl Pts',(-1.54529289749872,5.90374561007338,-1.38291033277678));
#6398=CARTESIAN_POINT('Ctrl Pts',(-1.09605031831592,6.11207894340678,-1.67659613043342));
#6399=CARTESIAN_POINT('Ctrl Pts',(-0.646807739133139,6.3204122767401,-1.97028192809006));
#6400=CARTESIAN_POINT('Ctrl Pts',(-0.110909354270905,6.52874561007347,-2.00000000000006));
#6401=CARTESIAN_POINT('Ctrl Pts',(0.424989030591338,6.73707894340672,-2.02971807190996));
#6402=CARTESIAN_POINT('Ctrl Pts',(0.903949681684068,6.94541227674014,-1.78750548470433));
#6403=CARTESIAN_POINT('Ctrl Pts',(1.38291033277681,7.15374561007342,-1.54529289749877));
#6404=CARTESIAN_POINT('Ctrl Pts',(1.6765961304334,7.36207894340677,-1.09605031831599));
#6405=CARTESIAN_POINT('Ctrl Pts',(1.97028192809006,7.57041227674011,-0.646807739133152));
#6406=CARTESIAN_POINT('Ctrl Pts',(2.,7.77874561007349,-0.110909354270917));
#6407=CARTESIAN_POINT('Ctrl Pts',(2.02971807190995,7.98707894340672,0.424989030591319));
#6408=CARTESIAN_POINT('Ctrl Pts',(1.78750548470433,8.19541227674012,0.903949681684058));
#6409=CARTESIAN_POINT('Ctrl Pts',(1.54529289749873,8.40374561007341,1.3829103327768));
#6410=CARTESIAN_POINT('Ctrl Pts',(1.09605031831593,8.6120789434068,1.67659613043337));
#6411=CARTESIAN_POINT('Ctrl Pts',(0.646807739133154,8.82041227674011,1.97028192809005));
#6412=CARTESIAN_POINT('Ctrl Pts',(0.110909354270904,9.02874561007346,1.99999999999994));
#6413=CARTESIAN_POINT('Ctrl Pts',(-0.424989030591337,9.23707894340678,2.02971807190995));
#6414=CARTESIAN_POINT('Ctrl Pts',(-0.903949681684064,9.44541227674011,1.78750548470427));
#6415=CARTESIAN_POINT('Ctrl Pts',(-1.38291033277679,9.65374561007344,1.54529289749871));
#6416=CARTESIAN_POINT('Ctrl Pts',(-1.67659613043342,9.86207894340678,1.09605031831593));
#6417=CARTESIAN_POINT('Ctrl Pts',(-1.97028192809005,10.0704122767401,0.646807739133152));
#6418=CARTESIAN_POINT('Ctrl Pts',(-1.99999999999999,10.2787456100735,0.110909354270841));
#6419=CARTESIAN_POINT('Ctrl Pts',(-2.02971807190994,10.4870789434068,-0.42498903059134));
#6420=CARTESIAN_POINT('Ctrl Pts',(-1.78750548470433,10.6954122767401,-0.903949681684169));
#6421=CARTESIAN_POINT('Ctrl Pts',(-1.54529289749871,10.9037456100734,-1.38291033277681));
#6422=CARTESIAN_POINT('Ctrl Pts',(-1.09605031831593,11.1120789434068,-1.67659613043348));
#6423=CARTESIAN_POINT('Ctrl Pts',(-0.646807739133152,11.3204122767401,-1.97028192809006));
#6424=CARTESIAN_POINT('Ctrl Pts',(-0.110909354270907,11.5287456100735,-2.00000000000002));
#6425=CARTESIAN_POINT('Ctrl Pts',(0.424989030591338,11.7370789434068,-2.02971807190997));
#6426=CARTESIAN_POINT('Ctrl Pts',(0.903949681684066,11.9454122767401,-1.78750548470433));
#6427=CARTESIAN_POINT('Ctrl Pts',(1.3829103327768,12.1537456100734,-1.54529289749877));
#6428=CARTESIAN_POINT('Ctrl Pts',(1.67659613043342,12.3620789434068,-1.09605031831594));
#6429=CARTESIAN_POINT('Ctrl Pts',(1.97028192809008,12.5704122767401,-0.646807739133166));
#6430=CARTESIAN_POINT('Ctrl Pts',(2.,12.7787456100735,-0.110909354270959));
#6431=CARTESIAN_POINT('Ctrl Pts',(2.02971807190995,12.9870789434068,0.42498903059134));
#6432=CARTESIAN_POINT('Ctrl Pts',(1.78750548470433,13.1954122767401,0.903949681684009));
#6433=CARTESIAN_POINT('Ctrl Pts',(1.54529289749872,13.4037456100734,1.38291033277679));
#6434=CARTESIAN_POINT('Ctrl Pts',(1.09605031831593,13.6120789434068,1.67659613043342));
#6435=CARTESIAN_POINT('Ctrl Pts',(0.646807739133154,13.8204122767401,1.97028192809006));
#6436=CARTESIAN_POINT('Ctrl Pts',(0.110909354270907,14.0287456100735,1.99999999999997));
#6437=CARTESIAN_POINT('Ctrl Pts',(-0.424989030591338,14.2370789434068,2.02971807190995));
#6438=CARTESIAN_POINT('Ctrl Pts',(-0.903949681684066,14.4454122767402,1.78750548470424));
#6439=CARTESIAN_POINT('Ctrl Pts',(-1.38291033277679,14.6537456100734,1.54529289749866));
#6440=CARTESIAN_POINT('Ctrl Pts',(-1.67659613043342,14.8620789434068,1.09605031831587));
#6441=CARTESIAN_POINT('Ctrl Pts',(-1.97028192809004,15.0704122767401,0.646807739133166));
#6442=CARTESIAN_POINT('Ctrl Pts',(-2.,15.2787456100735,0.110909354270848));
#6443=CARTESIAN_POINT('Ctrl Pts',(-2.02971807190995,15.4870789434068,-0.424989030591448));
#6444=CARTESIAN_POINT('Ctrl Pts',(-1.78750548470433,15.6954122767401,-0.903949681684079));
#6445=CARTESIAN_POINT('Ctrl Pts',(-1.54529289749872,15.9037456100734,-1.3829103327768));
#6446=CARTESIAN_POINT('Ctrl Pts',(-1.09605031831592,16.1120789434068,-1.67659613043346));
#6447=CARTESIAN_POINT('Ctrl Pts',(-0.646807739133152,16.3204122767401,-1.97028192809011));
#6448=CARTESIAN_POINT('Ctrl Pts',(-0.110909354270907,16.5287456100735,-2.00000000000005));
#6449=CARTESIAN_POINT('Ctrl Pts',(0.42498903059134,16.7370789434068,-2.02971807190995));
#6450=CARTESIAN_POINT('Ctrl Pts',(0.90394968168408,16.9454122767401,-1.78750548470433));
#6451=CARTESIAN_POINT('Ctrl Pts',(1.38291033277679,17.1537456100734,-1.54529289749872));
#6452=CARTESIAN_POINT('Ctrl Pts',(1.67659613043342,17.3620789434068,-1.09605031831599));
#6453=CARTESIAN_POINT('Ctrl Pts',(1.97028192809005,17.5704122767401,-0.646807739133152));
#6454=CARTESIAN_POINT('Ctrl Pts',(2.,17.7787456100735,-0.110909354270917));
#6455=CARTESIAN_POINT('Ctrl Pts',(2.02971807190995,17.9870789434068,0.424989030591283));
#6456=CARTESIAN_POINT('Ctrl Pts',(1.78750548470433,18.1954122767401,0.903949681684051));
#6457=CARTESIAN_POINT('Ctrl Pts',(1.54529289749873,18.4037456100734,1.3829103327768));
#6458=CARTESIAN_POINT('Ctrl Pts',(1.09605031831593,18.6120789434068,1.67659613043337));
#6459=CARTESIAN_POINT('Ctrl Pts',(0.646807739133154,18.8204122767401,1.97028192809005));
#6460=CARTESIAN_POINT('Ctrl Pts',(0.110909354270905,19.0287456100735,1.99999999999995));
#6461=CARTESIAN_POINT('Ctrl Pts',(-0.424989030591338,19.2370789434068,2.02971807190995));
#6462=CARTESIAN_POINT('Ctrl Pts',(-0.903949681684064,19.4454122767402,1.78750548470426));
#6463=CARTESIAN_POINT('Ctrl Pts',(-1.38291033277679,19.6537456100734,1.54529289749871));
#6464=CARTESIAN_POINT('Ctrl Pts',(-1.67659613043342,19.8620789434068,1.0960503183159));
#6465=CARTESIAN_POINT('Ctrl Pts',(-1.97028192809006,20.0704122767401,0.646807739133152));
#6466=CARTESIAN_POINT('Ctrl Pts',(-1.99999999999999,20.2787456100735,0.11090935427082));
#6467=CARTESIAN_POINT('Ctrl Pts',(-2.02971807190993,20.4870789434068,-0.424989030591398));
#6468=CARTESIAN_POINT('Ctrl Pts',(-1.78750548470433,20.6954122767402,-0.903949681684127));
#6469=CARTESIAN_POINT('Ctrl Pts',(-1.5452928974987,20.9037456100735,-1.38291033277683));
#6470=CARTESIAN_POINT('Ctrl Pts',(-1.09605031831595,21.1120789434068,-1.67659613043348));
#6471=CARTESIAN_POINT('Ctrl Pts',(-0.646807739133154,21.3204122767401,-1.97028192809006));
#6472=CARTESIAN_POINT('Ctrl Pts',(-0.110909354270907,21.5287456100735,-2.));
#6473=CARTESIAN_POINT('Ctrl Pts',(0.424989030591338,21.7370789434068,-2.02971807190994));
#6474=CARTESIAN_POINT('Ctrl Pts',(0.903949681684066,21.9454122767402,-1.78750548470436));
#6475=CARTESIAN_POINT('Ctrl Pts',(1.38291033277679,22.1537456100734,-1.54529289749877));
#6476=CARTESIAN_POINT('Ctrl Pts',(1.67659613043343,22.3620789434069,-1.09605031831595));
#6477=CARTESIAN_POINT('Ctrl Pts',(1.97028192809003,22.5704122767401,-0.646807739133152));
#6478=CARTESIAN_POINT('Ctrl Pts',(2.,22.7787456100735,-0.110909354270945));
#6479=CARTESIAN_POINT('Ctrl Pts',(2.02971807190997,22.9870789434068,0.42498903059134));
#6480=CARTESIAN_POINT('Ctrl Pts',(1.78750548470433,23.1954122767402,0.903949681684009));
#6481=CARTESIAN_POINT('Ctrl Pts',(1.54529289749872,23.4037456100734,1.38291033277679));
#6482=CARTESIAN_POINT('Ctrl Pts',(1.09605031831593,23.6120789434068,1.6765961304334));
#6483=CARTESIAN_POINT('Ctrl Pts',(0.646807739133168,23.8204122767401,1.97028192809006));
#6484=CARTESIAN_POINT('Ctrl Pts',(0.110909354270907,24.0287456100735,1.99999999999992));
#6485=CARTESIAN_POINT('Ctrl Pts',(-0.424989030591338,24.2370789434068,2.02971807190996));
#6486=CARTESIAN_POINT('Ctrl Pts',(-0.903949681684066,24.4454122767402,1.78750548470424));
#6487=CARTESIAN_POINT('Ctrl Pts',(-1.38291033277678,24.6537456100735,1.54529289749864));
#6488=CARTESIAN_POINT('Ctrl Pts',(-1.67659613043341,24.8620789434068,1.09605031831588));
#6489=CARTESIAN_POINT('Ctrl Pts',(-1.97028192809005,25.0704122767401,0.646807739133166));
#6490=CARTESIAN_POINT('Ctrl Pts',(-2.,25.2787456100735,0.110909354270855));
#6491=CARTESIAN_POINT('Ctrl Pts',(-2.02971807190995,25.4870789434068,-0.424989030591369));
#6492=CARTESIAN_POINT('Ctrl Pts',(-1.78750548470433,25.6954122767401,-0.903949681684079));
#6493=CARTESIAN_POINT('Ctrl Pts',(-1.54529289749871,25.9037456100735,-1.3829103327768));
#6494=CARTESIAN_POINT('Ctrl Pts',(-1.09605031831593,26.1120789434068,-1.67659613043345));
#6495=CARTESIAN_POINT('Ctrl Pts',(-0.646807739133152,26.3204122767401,-1.97028192809011));
#6496=CARTESIAN_POINT('Ctrl Pts',(-0.110909354270907,26.5287456100735,-2.00000000000004));
#6497=CARTESIAN_POINT('Ctrl Pts',(0.424989030591353,26.7370789434068,-2.02971807190995));
#6498=CARTESIAN_POINT('Ctrl Pts',(0.90394968168408,26.9454122767402,-1.78750548470438));
#6499=CARTESIAN_POINT('Ctrl Pts',(1.38291033277679,27.1537456100734,-1.54529289749872));
#6500=CARTESIAN_POINT('Ctrl Pts',(1.6765961304334,27.3620789434068,-1.09605031831597));
#6501=CARTESIAN_POINT('Ctrl Pts',(1.97028192809005,27.5704122767401,-0.64680773913318));
#6502=CARTESIAN_POINT('Ctrl Pts',(1.99999999999997,27.7787456100735,-0.110909354270911));
#6503=CARTESIAN_POINT('Ctrl Pts',(2.02971807190995,27.9870789434068,0.424989030591333));
#6504=CARTESIAN_POINT('Ctrl Pts',(1.78750548470433,28.1954122767402,0.903949681684037));
#6505=CARTESIAN_POINT('Ctrl Pts',(1.5452928974987,28.4037456100735,1.38291033277679));
#6506=CARTESIAN_POINT('Ctrl Pts',(1.09605031831593,28.6120789434068,1.67659613043337));
#6507=CARTESIAN_POINT('Ctrl Pts',(0.646807739133154,28.8204122767401,1.97028192809002));
#6508=CARTESIAN_POINT('Ctrl Pts',(0.110909354270921,29.0287456100735,1.99999999999997));
#6509=CARTESIAN_POINT('Ctrl Pts',(-0.424989030591338,29.2370789434068,2.02971807190995));
#6510=CARTESIAN_POINT('Ctrl Pts',(-0.903949681684064,29.4454122767402,1.78750548470427));
#6511=CARTESIAN_POINT('Ctrl Pts',(-1.38291033277679,29.6537456100735,1.54529289749868));
#6512=CARTESIAN_POINT('Ctrl Pts',(-1.67659613043342,29.8620789434068,1.09605031831586));
#6513=CARTESIAN_POINT('Ctrl Pts',(-1.97028192809005,30.0704122767401,0.646807739133123));
#6514=CARTESIAN_POINT('Ctrl Pts',(-2.,30.2787456100735,0.110909354270834));
#6515=CARTESIAN_POINT('Ctrl Pts',(-2.02971807190995,30.4870789434068,-0.424989030591398));
#6516=CARTESIAN_POINT('Ctrl Pts',(-1.78750548470432,30.6954122767402,-0.903949681684113));
#6517=CARTESIAN_POINT('Ctrl Pts',(-1.54529289749872,30.9037456100735,-1.38291033277676));
#6518=CARTESIAN_POINT('Ctrl Pts',(-1.09605031831593,31.1120789434068,-1.67659613043348));
#6519=CARTESIAN_POINT('Ctrl Pts',(-0.646807739133152,31.3204122767401,-1.97028192809006));
#6520=CARTESIAN_POINT('Ctrl Pts',(-0.110909354270905,31.5287456100735,-2.));
#6521=CARTESIAN_POINT('Ctrl Pts',(0.42498903059134,31.7370789434068,-2.02971807190996));
#6522=CARTESIAN_POINT('Ctrl Pts',(0.903949681684054,31.9454122767402,-1.78750548470435));
#6523=CARTESIAN_POINT('Ctrl Pts',(1.38291033277679,32.1537456100735,-1.54529289749877));
#6524=CARTESIAN_POINT('Ctrl Pts',(1.67659613043342,32.3620789434069,-1.09605031831598));
#6525=CARTESIAN_POINT('Ctrl Pts',(1.97028192809005,32.5704122767401,-0.646807739133152));
#6526=CARTESIAN_POINT('Ctrl Pts',(2.,32.7787456100735,-0.110909354270917));
#6527=CARTESIAN_POINT('Ctrl Pts',(2.02971807190995,32.9870789434069,0.424989030591311));
#6528=CARTESIAN_POINT('Ctrl Pts',(1.78750548470433,33.1954122767402,0.903949681684009));
#6529=CARTESIAN_POINT('Ctrl Pts',(1.54529289749872,33.4037456100734,1.38291033277681));
#6530=CARTESIAN_POINT('Ctrl Pts',(1.09605031831593,33.6120789434068,1.67659613043341));
#6531=CARTESIAN_POINT('Ctrl Pts',(0.646807739133154,33.8204122767401,1.97028192809006));
#6532=CARTESIAN_POINT('Ctrl Pts',(0.110909354270907,34.0287456100735,1.99999999999993));
#6533=CARTESIAN_POINT('Ctrl Pts',(-0.424989030591338,34.2370789434068,2.02971807190994));
#6534=CARTESIAN_POINT('Ctrl Pts',(-0.903949681684066,34.4454122767402,1.78750548470426));
#6535=CARTESIAN_POINT('Ctrl Pts',(-1.38291033277681,34.6537456100735,1.54529289749869));
#6536=CARTESIAN_POINT('Ctrl Pts',(-1.67659613043341,34.8620789434068,1.0960503183159));
#6537=CARTESIAN_POINT('Ctrl Pts',(-1.97028192809005,35.0704122767402,0.646807739133166));
#6538=CARTESIAN_POINT('Ctrl Pts',(-2.,35.2787456100736,0.110909354270855));
#6539=CARTESIAN_POINT('Ctrl Pts',(-2.02971807190995,35.4870789434068,-0.424989030591383));
#6540=CARTESIAN_POINT('Ctrl Pts',(-1.78750548470433,35.6954122767402,-0.903949681684099));
#6541=CARTESIAN_POINT('Ctrl Pts',(-1.54529289749872,35.9037456100735,-1.38291033277681));
#6542=CARTESIAN_POINT('Ctrl Pts',(-1.09605031831593,36.1120789434069,-1.67659613043344));
#6543=CARTESIAN_POINT('Ctrl Pts',(-0.646807739133139,36.3204122767402,-1.97028192809006));
#6544=CARTESIAN_POINT('Ctrl Pts',(-0.110909354270907,36.5287456100735,-2.00000000000004));
#6545=CARTESIAN_POINT('Ctrl Pts',(0.424989030591338,36.7370789434068,-2.02971807190996));
#6546=CARTESIAN_POINT('Ctrl Pts',(0.903949681684066,36.9454122767402,-1.78750548470439));
#6547=CARTESIAN_POINT('Ctrl Pts',(1.38291033277679,37.1537456100734,-1.54529289749872));
#6548=CARTESIAN_POINT('Ctrl Pts',(1.67659613043343,37.3620789434069,-1.09605031831598));
#6549=CARTESIAN_POINT('Ctrl Pts',(1.97028192809006,37.5704122767401,-0.646807739133152));
#6550=CARTESIAN_POINT('Ctrl Pts',(2.,37.7787456100735,-0.110909354270952));
#6551=CARTESIAN_POINT('Ctrl Pts',(2.02971807190997,37.9870789434069,0.424989030591333));
#6552=CARTESIAN_POINT('Ctrl Pts',(1.78750548470433,38.1954122767402,0.903949681684023));
#6553=CARTESIAN_POINT('Ctrl Pts',(1.54529289749872,38.4037456100734,1.3829103327768));
#6554=CARTESIAN_POINT('Ctrl Pts',(1.09605031831595,38.6120789434069,1.67659613043338));
#6555=CARTESIAN_POINT('Ctrl Pts',(0.646807739133154,38.8204122767402,1.97028192809006));
#6556=CARTESIAN_POINT('Ctrl Pts',(0.110909354270921,39.0287456100735,1.99999999999997));
#6557=CARTESIAN_POINT('Ctrl Pts',(-0.424989030591324,39.2370789434069,2.02971807190996));
#6558=CARTESIAN_POINT('Ctrl Pts',(-0.903949681684052,39.4454122767402,1.78750548470429));
#6559=CARTESIAN_POINT('Ctrl Pts',(-1.38291033277679,39.6537456100735,1.54529289749867));
#6560=CARTESIAN_POINT('Ctrl Pts',(-1.67659613043342,39.8620789434069,1.09605031831587));
#6561=CARTESIAN_POINT('Ctrl Pts',(-1.97028192809005,40.0704122767402,0.646807739133166));
#6562=CARTESIAN_POINT('Ctrl Pts',(-2.,40.2787456100735,0.110909354270834));
#6563=CARTESIAN_POINT('Ctrl Pts',(-1.40000000000002,0.278745610073447,0.110909354270819));
#6564=CARTESIAN_POINT('Ctrl Pts',(-1.42971807190993,0.487078943406762,-0.264219515132761));
#6565=CARTESIAN_POINT('Ctrl Pts',(-1.26789024243367,0.695412276740075,-0.603949681684109));
#6566=CARTESIAN_POINT('Ctrl Pts',(-1.10606241295736,0.903745610073446,-0.943679848235563));
#6567=CARTESIAN_POINT('Ctrl Pts',(-0.796050318315929,1.11207894340677,-1.1569808881628));
#6568=CARTESIAN_POINT('Ctrl Pts',(-0.486038223674453,1.3204122767401,-1.37028192809014));
#6569=CARTESIAN_POINT('Ctrl Pts',(-0.110909354270902,1.52874561007343,-1.40000000000009));
#6570=CARTESIAN_POINT('Ctrl Pts',(0.26421951513267,1.73707894340676,-1.42971807191003));
#6571=CARTESIAN_POINT('Ctrl Pts',(0.60394968168407,1.9454122767401,-1.26789024243367));
#6572=CARTESIAN_POINT('Ctrl Pts',(0.943679848235471,2.15374561007345,-1.10606241295738));
#6573=CARTESIAN_POINT('Ctrl Pts',(1.15698088816274,2.36207894340676,-0.796050318316012));
#6574=CARTESIAN_POINT('Ctrl Pts',(1.37028192809006,2.5704122767401,-0.486038223674555));
#6575=CARTESIAN_POINT('Ctrl Pts',(1.39999999999998,2.77874561007344,-0.110909354270902));
#6576=CARTESIAN_POINT('Ctrl Pts',(1.42971807190994,2.98707894340678,0.264219515132648));
#6577=CARTESIAN_POINT('Ctrl Pts',(1.26789024243366,3.19541227674007,0.60394968168399));
#6578=CARTESIAN_POINT('Ctrl Pts',(1.10606241295741,3.40374561007344,0.943679848235385));
#6579=CARTESIAN_POINT('Ctrl Pts',(0.796050318315931,3.61207894340678,1.15698088816276));
#6580=CARTESIAN_POINT('Ctrl Pts',(0.486038223674496,3.82041227674011,1.37028192808997));
#6581=CARTESIAN_POINT('Ctrl Pts',(0.110909354270899,4.02874561007344,1.4));
#6582=CARTESIAN_POINT('Ctrl Pts',(-0.264219515132648,4.23707894340677,1.42971807190986));
#6583=CARTESIAN_POINT('Ctrl Pts',(-0.603949681684091,4.44541227674011,1.2678902424336));
#6584=CARTESIAN_POINT('Ctrl Pts',(-0.943679848235468,4.65374561007345,1.1060624129573));
#6585=CARTESIAN_POINT('Ctrl Pts',(-1.15698088816278,4.86207894340679,0.796050318315845));
#6586=CARTESIAN_POINT('Ctrl Pts',(-1.37028192809003,5.07041227674011,0.486038223674474));
#6587=CARTESIAN_POINT('Ctrl Pts',(-1.40000000000002,5.27874561007345,0.110909354270819));
#6588=CARTESIAN_POINT('Ctrl Pts',(-1.42971807190992,5.4870789434068,-0.264219515132837));
#6589=CARTESIAN_POINT('Ctrl Pts',(-1.26789024243366,5.69541227674011,-0.603949681684078));
#6590=CARTESIAN_POINT('Ctrl Pts',(-1.10606241295738,5.90374561007345,-0.943679848235563));
#6591=CARTESIAN_POINT('Ctrl Pts',(-0.79605031831595,6.11207894340678,-1.15698088816284));
#6592=CARTESIAN_POINT('Ctrl Pts',(-0.486038223674474,6.32041227674012,-1.37028192809014));
#6593=CARTESIAN_POINT('Ctrl Pts',(-0.110909354270923,6.52874561007347,-1.40000000000009));
#6594=CARTESIAN_POINT('Ctrl Pts',(0.264219515132672,6.7370789434068,-1.42971807191003));
#6595=CARTESIAN_POINT('Ctrl Pts',(0.60394968168407,6.94541227674011,-1.26789024243367));
#6596=CARTESIAN_POINT('Ctrl Pts',(0.943679848235474,7.15374561007344,-1.10606241295738));
#6597=CARTESIAN_POINT('Ctrl Pts',(1.15698088816276,7.36207894340676,-0.796050318316012));
#6598=CARTESIAN_POINT('Ctrl Pts',(1.37028192809008,7.57041227674013,-0.486038223674566));
#6599=CARTESIAN_POINT('Ctrl Pts',(1.4,7.77874561007344,-0.110909354270902));
#6600=CARTESIAN_POINT('Ctrl Pts',(1.42971807190995,7.98707894340678,0.264219515132605));
#6601=CARTESIAN_POINT('Ctrl Pts',(1.26789024243366,8.19541227674011,0.603949681683985));
#6602=CARTESIAN_POINT('Ctrl Pts',(1.10606241295739,8.40374561007346,0.943679848235385));
#6603=CARTESIAN_POINT('Ctrl Pts',(0.796050318315911,8.6120789434068,1.15698088816276));
#6604=CARTESIAN_POINT('Ctrl Pts',(0.486038223674474,8.82041227674011,1.37028192809001));
#6605=CARTESIAN_POINT('Ctrl Pts',(0.110909354270881,9.02874561007344,1.4));
#6606=CARTESIAN_POINT('Ctrl Pts',(-0.264219515132648,9.23707894340678,1.42971807190988));
#6607=CARTESIAN_POINT('Ctrl Pts',(-0.603949681684091,9.44541227674012,1.26789024243366));
#6608=CARTESIAN_POINT('Ctrl Pts',(-0.943679848235471,9.65374561007344,1.1060624129573));
#6609=CARTESIAN_POINT('Ctrl Pts',(-1.15698088816276,9.86207894340679,0.796050318315845));
#6610=CARTESIAN_POINT('Ctrl Pts',(-1.37028192809006,10.0704122767401,0.486038223674393));
#6611=CARTESIAN_POINT('Ctrl Pts',(-1.40000000000002,10.2787456100734,0.110909354270819));
#6612=CARTESIAN_POINT('Ctrl Pts',(-1.42971807190993,10.4870789434068,-0.264219515132756));
#6613=CARTESIAN_POINT('Ctrl Pts',(-1.26789024243369,10.6954122767401,-0.60394968168412));
#6614=CARTESIAN_POINT('Ctrl Pts',(-1.10606241295736,10.9037456100735,-0.94367984823553));
#6615=CARTESIAN_POINT('Ctrl Pts',(-0.79605031831595,11.1120789434068,-1.15698088816285));
#6616=CARTESIAN_POINT('Ctrl Pts',(-0.486038223674453,11.3204122767401,-1.37028192809014));
#6617=CARTESIAN_POINT('Ctrl Pts',(-0.110909354270923,11.5287456100735,-1.40000000000009));
#6618=CARTESIAN_POINT('Ctrl Pts',(0.264219515132691,11.7370789434068,-1.42971807191005));
#6619=CARTESIAN_POINT('Ctrl Pts',(0.60394968168405,11.9454122767401,-1.26789024243367));
#6620=CARTESIAN_POINT('Ctrl Pts',(0.943679848235492,12.1537456100735,-1.10606241295747));
#6621=CARTESIAN_POINT('Ctrl Pts',(1.15698088816276,12.3620789434068,-0.796050318316012));
#6622=CARTESIAN_POINT('Ctrl Pts',(1.37028192809006,12.5704122767401,-0.48603822367456));
#6623=CARTESIAN_POINT('Ctrl Pts',(1.4,12.7787456100735,-0.110909354270902));
#6624=CARTESIAN_POINT('Ctrl Pts',(1.42971807190997,12.9870789434068,0.264219515132578));
#6625=CARTESIAN_POINT('Ctrl Pts',(1.26789024243366,13.1954122767402,0.603949681683979));
#6626=CARTESIAN_POINT('Ctrl Pts',(1.10606241295738,13.4037456100734,0.943679848235428));
#6627=CARTESIAN_POINT('Ctrl Pts',(0.796050318315911,13.6120789434068,1.15698088816276));
#6628=CARTESIAN_POINT('Ctrl Pts',(0.486038223674477,13.8204122767401,1.37028192809001));
#6629=CARTESIAN_POINT('Ctrl Pts',(0.110909354270902,14.0287456100735,1.4));
#6630=CARTESIAN_POINT('Ctrl Pts',(-0.264219515132648,14.2370789434068,1.42971807190986));
#6631=CARTESIAN_POINT('Ctrl Pts',(-0.603949681684091,14.4454122767401,1.26789024243366));
#6632=CARTESIAN_POINT('Ctrl Pts',(-0.943679848235471,14.6537456100735,1.10606241295732));
#6633=CARTESIAN_POINT('Ctrl Pts',(-1.15698088816278,14.8620789434068,0.796050318315845));
#6634=CARTESIAN_POINT('Ctrl Pts',(-1.37028192809005,15.0704122767401,0.48603822367442));
#6635=CARTESIAN_POINT('Ctrl Pts',(-1.4,15.2787456100735,0.110909354270819));
#6636=CARTESIAN_POINT('Ctrl Pts',(-1.42971807190992,15.4870789434068,-0.264219515132718));
#6637=CARTESIAN_POINT('Ctrl Pts',(-1.26789024243366,15.6954122767401,-0.603949681684167));
#6638=CARTESIAN_POINT('Ctrl Pts',(-1.10606241295736,15.9037456100735,-0.943679848235573));
#6639=CARTESIAN_POINT('Ctrl Pts',(-0.796050318315929,16.1120789434068,-1.15698088816286));
#6640=CARTESIAN_POINT('Ctrl Pts',(-0.486038223674453,16.3204122767402,-1.37028192809016));
#6641=CARTESIAN_POINT('Ctrl Pts',(-0.110909354270902,16.5287456100735,-1.40000000000009));
#6642=CARTESIAN_POINT('Ctrl Pts',(0.264219515132672,16.7370789434068,-1.42971807191007));
#6643=CARTESIAN_POINT('Ctrl Pts',(0.60394968168407,16.9454122767402,-1.26789024243367));
#6644=CARTESIAN_POINT('Ctrl Pts',(0.943679848235471,17.1537456100735,-1.10606241295741));
#6645=CARTESIAN_POINT('Ctrl Pts',(1.15698088816274,17.3620789434068,-0.796050318316007));
#6646=CARTESIAN_POINT('Ctrl Pts',(1.37028192809005,17.5704122767402,-0.486038223674528));
#6647=CARTESIAN_POINT('Ctrl Pts',(1.39999999999998,17.7787456100735,-0.110909354270907));
#6648=CARTESIAN_POINT('Ctrl Pts',(1.42971807190994,17.9870789434068,0.2642195151326));
#6649=CARTESIAN_POINT('Ctrl Pts',(1.26789024243364,18.1954122767402,0.603949681683979));
#6650=CARTESIAN_POINT('Ctrl Pts',(1.10606241295739,18.4037456100735,0.943679848235406));
#6651=CARTESIAN_POINT('Ctrl Pts',(0.796050318315929,18.6120789434068,1.15698088816276));
#6652=CARTESIAN_POINT('Ctrl Pts',(0.486038223674496,18.8204122767402,1.37028192808999));
#6653=CARTESIAN_POINT('Ctrl Pts',(0.110909354270902,19.0287456100735,1.39999999999996));
#6654=CARTESIAN_POINT('Ctrl Pts',(-0.26421951513267,19.2370789434068,1.42971807190988));
#6655=CARTESIAN_POINT('Ctrl Pts',(-0.60394968168407,19.4454122767402,1.26789024243363));
#6656=CARTESIAN_POINT('Ctrl Pts',(-0.943679848235452,19.6537456100735,1.1060624129573));
#6657=CARTESIAN_POINT('Ctrl Pts',(-1.15698088816278,19.8620789434068,0.796050318315845));
#6658=CARTESIAN_POINT('Ctrl Pts',(-1.37028192809005,20.0704122767402,0.486038223674393));
#6659=CARTESIAN_POINT('Ctrl Pts',(-1.4,20.2787456100735,0.110909354270813));
#6660=CARTESIAN_POINT('Ctrl Pts',(-1.42971807190994,20.4870789434068,-0.26421951513274));
#6661=CARTESIAN_POINT('Ctrl Pts',(-1.26789024243366,20.6954122767402,-0.603949681684167));
#6662=CARTESIAN_POINT('Ctrl Pts',(-1.10606241295736,20.9037456100735,-0.943679848235573));
#6663=CARTESIAN_POINT('Ctrl Pts',(-0.79605031831595,21.1120789434068,-1.15698088816285));
#6664=CARTESIAN_POINT('Ctrl Pts',(-0.486038223674453,21.3204122767402,-1.37028192809015));
#6665=CARTESIAN_POINT('Ctrl Pts',(-0.110909354270923,21.5287456100735,-1.4000000000001));
#6666=CARTESIAN_POINT('Ctrl Pts',(0.264219515132691,21.7370789434068,-1.42971807191004));
#6667=CARTESIAN_POINT('Ctrl Pts',(0.60394968168407,21.9454122767402,-1.26789024243367));
#6668=CARTESIAN_POINT('Ctrl Pts',(0.943679848235474,22.1537456100735,-1.10606241295747));
#6669=CARTESIAN_POINT('Ctrl Pts',(1.15698088816276,22.3620789434068,-0.796050318316001));
#6670=CARTESIAN_POINT('Ctrl Pts',(1.37028192809006,22.5704122767402,-0.486038223674555));
#6671=CARTESIAN_POINT('Ctrl Pts',(1.4,22.7787456100735,-0.110909354270928));
#6672=CARTESIAN_POINT('Ctrl Pts',(1.42971807190997,22.9870789434068,0.264219515132573));
#6673=CARTESIAN_POINT('Ctrl Pts',(1.26789024243366,23.1954122767402,0.603949681684057));
#6674=CARTESIAN_POINT('Ctrl Pts',(1.10606241295738,23.4037456100735,0.943679848235433));
#6675=CARTESIAN_POINT('Ctrl Pts',(0.796050318315926,23.6120789434068,1.15698088816273));
#6676=CARTESIAN_POINT('Ctrl Pts',(0.486038223674474,23.8204122767402,1.37028192809002));
#6677=CARTESIAN_POINT('Ctrl Pts',(0.110909354270881,24.0287456100735,1.39999999999998));
#6678=CARTESIAN_POINT('Ctrl Pts',(-0.264219515132651,24.2370789434069,1.42971807190985));
#6679=CARTESIAN_POINT('Ctrl Pts',(-0.603949681684091,24.4454122767401,1.2678902424336));
#6680=CARTESIAN_POINT('Ctrl Pts',(-0.943679848235471,24.6537456100735,1.10606241295733));
#6681=CARTESIAN_POINT('Ctrl Pts',(-1.15698088816276,24.8620789434068,0.796050318315887));
#6682=CARTESIAN_POINT('Ctrl Pts',(-1.37028192809005,25.0704122767401,0.486038223674404));
#6683=CARTESIAN_POINT('Ctrl Pts',(-1.4,25.2787456100735,0.110909354270813));
#6684=CARTESIAN_POINT('Ctrl Pts',(-1.42971807190994,25.4870789434068,-0.264219515132734));
#6685=CARTESIAN_POINT('Ctrl Pts',(-1.26789024243369,25.6954122767402,-0.603949681684162));
#6686=CARTESIAN_POINT('Ctrl Pts',(-1.10606241295738,25.9037456100735,-0.943679848235541));
#6687=CARTESIAN_POINT('Ctrl Pts',(-0.79605031831595,26.1120789434068,-1.15698088816286));
#6688=CARTESIAN_POINT('Ctrl Pts',(-0.486038223674453,26.3204122767402,-1.37028192809015));
#6689=CARTESIAN_POINT('Ctrl Pts',(-0.110909354270923,26.5287456100735,-1.4000000000001));
#6690=CARTESIAN_POINT('Ctrl Pts',(0.264219515132694,26.7370789434069,-1.42971807191004));
#6691=CARTESIAN_POINT('Ctrl Pts',(0.60394968168405,26.9454122767402,-1.26789024243367));
#6692=CARTESIAN_POINT('Ctrl Pts',(0.943679848235492,27.1537456100735,-1.10606241295747));
#6693=CARTESIAN_POINT('Ctrl Pts',(1.15698088816274,27.3620789434069,-0.796050318316001));
#6694=CARTESIAN_POINT('Ctrl Pts',(1.37028192809008,27.5704122767402,-0.486038223674528));
#6695=CARTESIAN_POINT('Ctrl Pts',(1.39999999999998,27.7787456100735,-0.110909354270917));
#6696=CARTESIAN_POINT('Ctrl Pts',(1.42971807190997,27.9870789434068,0.264219515132594));
#6697=CARTESIAN_POINT('Ctrl Pts',(1.26789024243366,28.1954122767402,0.603949681684047));
#6698=CARTESIAN_POINT('Ctrl Pts',(1.10606241295738,28.4037456100735,0.943679848235406));
#6699=CARTESIAN_POINT('Ctrl Pts',(0.796050318315908,28.6120789434068,1.15698088816274));
#6700=CARTESIAN_POINT('Ctrl Pts',(0.486038223674496,28.8204122767402,1.37028192809));
#6701=CARTESIAN_POINT('Ctrl Pts',(0.110909354270902,29.0287456100735,1.39999999999997));
#6702=CARTESIAN_POINT('Ctrl Pts',(-0.26421951513267,29.2370789434068,1.42971807190989));
#6703=CARTESIAN_POINT('Ctrl Pts',(-0.603949681684091,29.4454122767402,1.26789024243359));
#6704=CARTESIAN_POINT('Ctrl Pts',(-0.943679848235452,29.6537456100735,1.10606241295731));
#6705=CARTESIAN_POINT('Ctrl Pts',(-1.15698088816278,29.8620789434069,0.796050318315892));
#6706=CARTESIAN_POINT('Ctrl Pts',(-1.37028192809005,30.0704122767402,0.486038223674393));
#6707=CARTESIAN_POINT('Ctrl Pts',(-1.4,30.2787456100735,0.11090935427086));
#6708=CARTESIAN_POINT('Ctrl Pts',(-1.42971807190994,30.4870789434069,-0.26421951513274));
#6709=CARTESIAN_POINT('Ctrl Pts',(-1.26789024243366,30.6954122767402,-0.603949681684162));
#6710=CARTESIAN_POINT('Ctrl Pts',(-1.10606241295736,30.9037456100735,-0.943679848235563));
#6711=CARTESIAN_POINT('Ctrl Pts',(-0.79605031831595,31.1120789434068,-1.15698088816285));
#6712=CARTESIAN_POINT('Ctrl Pts',(-0.486038223674471,31.3204122767402,-1.37028192809016));
#6713=CARTESIAN_POINT('Ctrl Pts',(-0.110909354270923,31.5287456100735,-1.4000000000001));
#6714=CARTESIAN_POINT('Ctrl Pts',(0.264219515132691,31.7370789434069,-1.42971807191));
#6715=CARTESIAN_POINT('Ctrl Pts',(0.60394968168407,31.9454122767402,-1.26789024243368));
#6716=CARTESIAN_POINT('Ctrl Pts',(0.943679848235474,32.1537456100735,-1.10606241295744));
#6717=CARTESIAN_POINT('Ctrl Pts',(1.15698088816274,32.3620789434069,-0.796050318315981));
#6718=CARTESIAN_POINT('Ctrl Pts',(1.37028192809005,32.5704122767402,-0.48603822367455));
#6719=CARTESIAN_POINT('Ctrl Pts',(1.4,32.7787456100735,-0.110909354270917));
#6720=CARTESIAN_POINT('Ctrl Pts',(1.42971807190994,32.9870789434069,0.264219515132578));
#6721=CARTESIAN_POINT('Ctrl Pts',(1.26789024243364,33.1954122767402,0.603949681684047));
#6722=CARTESIAN_POINT('Ctrl Pts',(1.10606241295741,33.4037456100735,0.943679848235428));
#6723=CARTESIAN_POINT('Ctrl Pts',(0.796050318315929,33.6120789434069,1.15698088816274));
#6724=CARTESIAN_POINT('Ctrl Pts',(0.486038223674496,33.8204122767402,1.37028192809002));
#6725=CARTESIAN_POINT('Ctrl Pts',(0.110909354270881,34.0287456100735,1.39999999999998));
#6726=CARTESIAN_POINT('Ctrl Pts',(-0.26421951513267,34.2370789434069,1.42971807190985));
#6727=CARTESIAN_POINT('Ctrl Pts',(-0.603949681684091,34.4454122767402,1.26789024243359));
#6728=CARTESIAN_POINT('Ctrl Pts',(-0.943679848235449,34.6537456100735,1.10606241295733));
#6729=CARTESIAN_POINT('Ctrl Pts',(-1.15698088816278,34.8620789434069,0.796050318315903));
#6730=CARTESIAN_POINT('Ctrl Pts',(-1.37028192809003,35.0704122767402,0.486038223674404));
#6731=CARTESIAN_POINT('Ctrl Pts',(-1.4,35.2787456100735,0.11090935427086));
#6732=CARTESIAN_POINT('Ctrl Pts',(-1.42971807190994,35.4870789434069,-0.264219515132756));
#6733=CARTESIAN_POINT('Ctrl Pts',(-1.26789024243369,35.6954122767402,-0.603949681684089));
#6734=CARTESIAN_POINT('Ctrl Pts',(-1.10606241295738,35.9037456100736,-0.943679848235563));
#6735=CARTESIAN_POINT('Ctrl Pts',(-0.79605031831595,36.1120789434069,-1.15698088816278));
#6736=CARTESIAN_POINT('Ctrl Pts',(-0.486038223674474,36.3204122767402,-1.37028192809014));
#6737=CARTESIAN_POINT('Ctrl Pts',(-0.11090935427092,36.5287456100735,-1.40000000000009));
#6738=CARTESIAN_POINT('Ctrl Pts',(0.264219515132672,36.7370789434069,-1.42971807191003));
#6739=CARTESIAN_POINT('Ctrl Pts',(0.60394968168405,36.9454122767402,-1.2678902424337));
#6740=CARTESIAN_POINT('Ctrl Pts',(0.943679848235492,37.1537456100735,-1.10606241295747));
#6741=CARTESIAN_POINT('Ctrl Pts',(1.15698088816274,37.3620789434068,-0.796050318315981));
#6742=CARTESIAN_POINT('Ctrl Pts',(1.37028192809008,37.5704122767402,-0.486038223674555));
#6743=CARTESIAN_POINT('Ctrl Pts',(1.4,37.7787456100735,-0.110909354270923));
#6744=CARTESIAN_POINT('Ctrl Pts',(1.42971807190994,37.9870789434069,0.264219515132605));
#6745=CARTESIAN_POINT('Ctrl Pts',(1.26789024243366,38.1954122767402,0.603949681684011));
#6746=CARTESIAN_POINT('Ctrl Pts',(1.10606241295738,38.4037456100735,0.943679848235417));
#6747=CARTESIAN_POINT('Ctrl Pts',(0.796050318315929,38.6120789434069,1.15698088816273));
#6748=CARTESIAN_POINT('Ctrl Pts',(0.486038223674474,38.8204122767402,1.37028192808999));
#6749=CARTESIAN_POINT('Ctrl Pts',(0.110909354270881,39.0287456100735,1.39999999999998));
#6750=CARTESIAN_POINT('Ctrl Pts',(-0.264219515132648,39.2370789434069,1.42971807190988));
#6751=CARTESIAN_POINT('Ctrl Pts',(-0.603949681684073,39.4454122767402,1.26789024243359));
#6752=CARTESIAN_POINT('Ctrl Pts',(-0.943679848235474,39.6537456100736,1.10606241295731));
#6753=CARTESIAN_POINT('Ctrl Pts',(-1.15698088816278,39.8620789434069,0.796050318315897));
#6754=CARTESIAN_POINT('Ctrl Pts',(-1.37028192809005,40.0704122767402,0.486038223674399));
#6755=CARTESIAN_POINT('Ctrl Pts',(-1.4,40.2787456100735,0.11090935427086));
#6756=CARTESIAN_POINT('Ctrl Pts',(-1.4,-0.278745610073483,-0.110909354270949));
#6757=CARTESIAN_POINT('Ctrl Pts',(-1.37028192809006,-0.0704122767401418,
-0.486038223674447));
#6758=CARTESIAN_POINT('Ctrl Pts',(-1.1569808881628,0.137921056593191,-0.796050318316017));
#6759=CARTESIAN_POINT('Ctrl Pts',(-0.943679848235495,0.346254389926559,
-1.10606241295736));
#6760=CARTESIAN_POINT('Ctrl Pts',(-0.60394968168412,0.554587723259871,-1.26789024243366));
#6761=CARTESIAN_POINT('Ctrl Pts',(-0.264219515132702,0.762921056593206,
-1.42971807191002));
#6762=CARTESIAN_POINT('Ctrl Pts',(0.11090935427085,0.971254389926519,-1.39999999999999));
#6763=CARTESIAN_POINT('Ctrl Pts',(0.486038223674463,1.17958772325989,-1.37028192809015));
#6764=CARTESIAN_POINT('Ctrl Pts',(0.7960503183159,1.3879210565932,-1.15698088816281));
#6765=CARTESIAN_POINT('Ctrl Pts',(1.10606241295738,1.59625438992658,-0.943679848235584));
#6766=CARTESIAN_POINT('Ctrl Pts',(1.26789024243364,1.80458772325987,-0.603949681684177));
#6767=CARTESIAN_POINT('Ctrl Pts',(1.42971807190996,2.01292105659321,-0.264219515132788));
#6768=CARTESIAN_POINT('Ctrl Pts',(1.39999999999998,2.22125438992654,0.110909354270787));
#6769=CARTESIAN_POINT('Ctrl Pts',(1.37028192809009,2.42958772325987,0.486038223674361));
#6770=CARTESIAN_POINT('Ctrl Pts',(1.15698088816276,2.63792105659322,0.796050318315897));
#6771=CARTESIAN_POINT('Ctrl Pts',(0.943679848235517,2.84625438992656,1.10606241295735));
#6772=CARTESIAN_POINT('Ctrl Pts',(0.603949681684099,3.05458772325989,1.26789024243365));
#6773=CARTESIAN_POINT('Ctrl Pts',(0.264219515132705,3.26292105659324,1.42971807190985));
#6774=CARTESIAN_POINT('Ctrl Pts',(-0.110909354270889,3.47125438992654,1.39999999999992));
#6775=CARTESIAN_POINT('Ctrl Pts',(-0.48603822367442,3.67958772325988,1.37028192808998));
#6776=CARTESIAN_POINT('Ctrl Pts',(-0.796050318315921,3.8879210565932,1.15698088816272));
#6777=CARTESIAN_POINT('Ctrl Pts',(-1.10606241295734,4.09625438992655,0.943679848235406));
#6778=CARTESIAN_POINT('Ctrl Pts',(-1.26789024243365,4.30458772325989,0.603949681684094));
#6779=CARTESIAN_POINT('Ctrl Pts',(-1.42971807190994,4.51292105659323,0.2642195151326));
#6780=CARTESIAN_POINT('Ctrl Pts',(-1.4,4.72125438992655,-0.110909354270949));
#6781=CARTESIAN_POINT('Ctrl Pts',(-1.37028192809004,4.9295877232599,-0.486038223674442));
#6782=CARTESIAN_POINT('Ctrl Pts',(-1.15698088816278,5.13792105659321,-0.796050318315991));
#6783=CARTESIAN_POINT('Ctrl Pts',(-0.943679848235495,5.34625438992658,-1.10606241295745));
#6784=CARTESIAN_POINT('Ctrl Pts',(-0.603949681684099,5.55458772325993,-1.26789024243366));
#6785=CARTESIAN_POINT('Ctrl Pts',(-0.264219515132702,5.76292105659326,-1.42971807190998));
#6786=CARTESIAN_POINT('Ctrl Pts',(0.110909354270868,5.97125438992656,-1.40000000000003));
#6787=CARTESIAN_POINT('Ctrl Pts',(0.486038223674442,6.17958772325989,-1.37028192809015));
#6788=CARTESIAN_POINT('Ctrl Pts',(0.796050318315879,6.38792105659323,-1.15698088816278));
#6789=CARTESIAN_POINT('Ctrl Pts',(1.10606241295736,6.59625438992658,-0.943679848235606));
#6790=CARTESIAN_POINT('Ctrl Pts',(1.26789024243365,6.80458772325986,-0.603949681684177));
#6791=CARTESIAN_POINT('Ctrl Pts',(1.42971807190994,7.01292105659325,-0.264219515132794));
#6792=CARTESIAN_POINT('Ctrl Pts',(1.4,7.22125438992654,0.110909354270824));
#6793=CARTESIAN_POINT('Ctrl Pts',(1.37028192809007,7.42958772325991,0.486038223674361));
#6794=CARTESIAN_POINT('Ctrl Pts',(1.15698088816276,7.63792105659323,0.796050318315897));
#6795=CARTESIAN_POINT('Ctrl Pts',(0.943679848235498,7.84625438992655,1.10606241295728));
#6796=CARTESIAN_POINT('Ctrl Pts',(0.603949681684078,8.05458772325989,1.26789024243365));
#6797=CARTESIAN_POINT('Ctrl Pts',(0.264219515132724,8.26292105659323,1.42971807190989));
#6798=CARTESIAN_POINT('Ctrl Pts',(-0.110909354270889,8.47125438992655,1.39999999999992));
#6799=CARTESIAN_POINT('Ctrl Pts',(-0.486038223674439,8.67958772325992,1.37028192808998));
#6800=CARTESIAN_POINT('Ctrl Pts',(-0.796050318315921,8.88792105659323,1.15698088816273));
#6801=CARTESIAN_POINT('Ctrl Pts',(-1.10606241295736,9.09625438992657,0.94367984823539));
#6802=CARTESIAN_POINT('Ctrl Pts',(-1.26789024243365,9.3045877232599,0.603949681684094));
#6803=CARTESIAN_POINT('Ctrl Pts',(-1.42971807190994,9.51292105659322,0.264219515132616));
#6804=CARTESIAN_POINT('Ctrl Pts',(-1.4,9.72125438992658,-0.110909354270954));
#6805=CARTESIAN_POINT('Ctrl Pts',(-1.37028192809006,9.92958772325988,-0.486038223674523));
#6806=CARTESIAN_POINT('Ctrl Pts',(-1.1569808881628,10.1379210565933,-0.796050318315991));
#6807=CARTESIAN_POINT('Ctrl Pts',(-0.943679848235474,10.3462543899266,-1.10606241295745));
#6808=CARTESIAN_POINT('Ctrl Pts',(-0.60394968168412,10.5545877232599,-1.26789024243366));
#6809=CARTESIAN_POINT('Ctrl Pts',(-0.264219515132683,10.7629210565932,-1.42971807191006));
#6810=CARTESIAN_POINT('Ctrl Pts',(0.110909354270847,10.9712543899266,-1.40000000000007));
#6811=CARTESIAN_POINT('Ctrl Pts',(0.486038223674463,11.1795877232599,-1.37028192809018));
#6812=CARTESIAN_POINT('Ctrl Pts',(0.7960503183159,11.3879210565933,-1.15698088816279));
#6813=CARTESIAN_POINT('Ctrl Pts',(1.10606241295736,11.5962543899266,-0.943679848235595));
#6814=CARTESIAN_POINT('Ctrl Pts',(1.26789024243365,11.8045877232599,-0.603949681684188));
#6815=CARTESIAN_POINT('Ctrl Pts',(1.42971807190994,12.0129210565932,-0.264219515132707));
#6816=CARTESIAN_POINT('Ctrl Pts',(1.4,12.2212543899266,0.110909354270855));
#6817=CARTESIAN_POINT('Ctrl Pts',(1.37028192809006,12.4295877232599,0.486038223674382));
#6818=CARTESIAN_POINT('Ctrl Pts',(1.15698088816276,12.6379210565932,0.796050318315897));
#6819=CARTESIAN_POINT('Ctrl Pts',(0.943679848235517,12.8462543899266,1.10606241295731));
#6820=CARTESIAN_POINT('Ctrl Pts',(0.603949681684099,13.0545877232599,1.26789024243365));
#6821=CARTESIAN_POINT('Ctrl Pts',(0.264219515132705,13.2629210565933,1.42971807190989));
#6822=CARTESIAN_POINT('Ctrl Pts',(-0.110909354270889,13.4712543899266,1.39999999999992));
#6823=CARTESIAN_POINT('Ctrl Pts',(-0.48603822367442,13.6795877232599,1.37028192808998));
#6824=CARTESIAN_POINT('Ctrl Pts',(-0.7960503183159,13.8879210565933,1.15698088816275));
#6825=CARTESIAN_POINT('Ctrl Pts',(-1.10606241295736,14.0962543899266,0.943679848235428));
#6826=CARTESIAN_POINT('Ctrl Pts',(-1.26789024243365,14.3045877232599,0.603949681684078));
#6827=CARTESIAN_POINT('Ctrl Pts',(-1.42971807190992,14.5129210565933,0.264219515132632));
#6828=CARTESIAN_POINT('Ctrl Pts',(-1.40000000000002,14.7212543899266,-0.110909354270954));
#6829=CARTESIAN_POINT('Ctrl Pts',(-1.37028192809007,14.9295877232599,-0.486038223674463));
#6830=CARTESIAN_POINT('Ctrl Pts',(-1.15698088816278,15.1379210565933,-0.796050318315991));
#6831=CARTESIAN_POINT('Ctrl Pts',(-0.943679848235495,15.3462543899266,-1.10606241295744));
#6832=CARTESIAN_POINT('Ctrl Pts',(-0.60394968168412,15.55458772326,-1.26789024243366));
#6833=CARTESIAN_POINT('Ctrl Pts',(-0.264219515132702,15.7629210565933,-1.42971807191003));
#6834=CARTESIAN_POINT('Ctrl Pts',(0.110909354270868,15.9712543899266,-1.40000000000008));
#6835=CARTESIAN_POINT('Ctrl Pts',(0.486038223674463,16.1795877232599,-1.37028192809016));
#6836=CARTESIAN_POINT('Ctrl Pts',(0.796050318315879,16.3879210565933,-1.15698088816279));
#6837=CARTESIAN_POINT('Ctrl Pts',(1.10606241295736,16.5962543899266,-0.94367984823559));
#6838=CARTESIAN_POINT('Ctrl Pts',(1.26789024243365,16.8045877232599,-0.603949681684188));
#6839=CARTESIAN_POINT('Ctrl Pts',(1.42971807190996,17.0129210565933,-0.264219515132783));
#6840=CARTESIAN_POINT('Ctrl Pts',(1.39999999999998,17.2212543899266,0.11090935427085));
#6841=CARTESIAN_POINT('Ctrl Pts',(1.37028192809007,17.4295877232599,0.486038223674382));
#6842=CARTESIAN_POINT('Ctrl Pts',(1.15698088816276,17.6379210565933,0.796050318315892));
#6843=CARTESIAN_POINT('Ctrl Pts',(0.943679848235517,17.8462543899266,1.10606241295728));
#6844=CARTESIAN_POINT('Ctrl Pts',(0.603949681684099,18.0545877232599,1.26789024243363));
#6845=CARTESIAN_POINT('Ctrl Pts',(0.264219515132724,18.2629210565933,1.42971807190987));
#6846=CARTESIAN_POINT('Ctrl Pts',(-0.110909354270889,18.4712543899266,1.39999999999997));
#6847=CARTESIAN_POINT('Ctrl Pts',(-0.48603822367442,18.6795877232599,1.37028192808996));
#6848=CARTESIAN_POINT('Ctrl Pts',(-0.796050318315921,18.8879210565933,1.15698088816276));
#6849=CARTESIAN_POINT('Ctrl Pts',(-1.10606241295736,19.0962543899266,0.943679848235417));
#6850=CARTESIAN_POINT('Ctrl Pts',(-1.26789024243365,19.3045877232599,0.603949681684037));
#6851=CARTESIAN_POINT('Ctrl Pts',(-1.42971807190994,19.5129210565933,0.264219515132616));
#6852=CARTESIAN_POINT('Ctrl Pts',(-1.4,19.7212543899266,-0.110909354270954));
#6853=CARTESIAN_POINT('Ctrl Pts',(-1.37028192809006,19.9295877232599,-0.486038223674496));
#6854=CARTESIAN_POINT('Ctrl Pts',(-1.1569808881628,20.1379210565933,-0.796050318315996));
#6855=CARTESIAN_POINT('Ctrl Pts',(-0.943679848235474,20.3462543899266,-1.10606241295739));
#6856=CARTESIAN_POINT('Ctrl Pts',(-0.603949681684099,20.5545877232599,-1.26789024243366));
#6857=CARTESIAN_POINT('Ctrl Pts',(-0.264219515132683,20.7629210565933,-1.42971807191002));
#6858=CARTESIAN_POINT('Ctrl Pts',(0.110909354270868,20.9712543899266,-1.40000000000009));
#6859=CARTESIAN_POINT('Ctrl Pts',(0.486038223674463,21.1795877232599,-1.37028192809016));
#6860=CARTESIAN_POINT('Ctrl Pts',(0.796050318315879,21.3879210565933,-1.15698088816278));
#6861=CARTESIAN_POINT('Ctrl Pts',(1.10606241295736,21.5962543899266,-0.943679848235579));
#6862=CARTESIAN_POINT('Ctrl Pts',(1.26789024243365,21.8045877232599,-0.603949681684177));
#6863=CARTESIAN_POINT('Ctrl Pts',(1.42971807190994,22.0129210565933,-0.264219515132783));
#6864=CARTESIAN_POINT('Ctrl Pts',(1.4,22.2212543899266,0.110909354270855));
#6865=CARTESIAN_POINT('Ctrl Pts',(1.37028192809006,22.42958772326,0.486038223674372));
#6866=CARTESIAN_POINT('Ctrl Pts',(1.15698088816276,22.6379210565933,0.796050318315892));
#6867=CARTESIAN_POINT('Ctrl Pts',(0.943679848235495,22.8462543899266,1.10606241295731));
#6868=CARTESIAN_POINT('Ctrl Pts',(0.603949681684078,23.0545877232599,1.26789024243363));
#6869=CARTESIAN_POINT('Ctrl Pts',(0.264219515132726,23.2629210565933,1.42971807190989));
#6870=CARTESIAN_POINT('Ctrl Pts',(-0.110909354270889,23.4712543899266,1.39999999999997));
#6871=CARTESIAN_POINT('Ctrl Pts',(-0.48603822367442,23.6795877232599,1.37028192808997));
#6872=CARTESIAN_POINT('Ctrl Pts',(-0.796050318315921,23.8879210565932,1.15698088816274));
#6873=CARTESIAN_POINT('Ctrl Pts',(-1.10606241295736,24.0962543899266,0.943679848235433));
#6874=CARTESIAN_POINT('Ctrl Pts',(-1.26789024243367,24.3045877232599,0.603949681684089));
#6875=CARTESIAN_POINT('Ctrl Pts',(-1.42971807190992,24.5129210565933,0.264219515132643));
#6876=CARTESIAN_POINT('Ctrl Pts',(-1.40000000000002,24.7212543899266,-0.110909354270923));
#6877=CARTESIAN_POINT('Ctrl Pts',(-1.37028192809004,24.9295877232599,-0.486038223674528));
#6878=CARTESIAN_POINT('Ctrl Pts',(-1.1569808881628,25.1379210565933,-0.796050318315996));
#6879=CARTESIAN_POINT('Ctrl Pts',(-0.943679848235474,25.3462543899266,-1.10606241295742));
#6880=CARTESIAN_POINT('Ctrl Pts',(-0.60394968168412,25.5545877232599,-1.26789024243365));
#6881=CARTESIAN_POINT('Ctrl Pts',(-0.264219515132702,25.7629210565933,-1.42971807191003));
#6882=CARTESIAN_POINT('Ctrl Pts',(0.110909354270847,25.9712543899266,-1.40000000000008));
#6883=CARTESIAN_POINT('Ctrl Pts',(0.486038223674463,26.17958772326,-1.37028192809014));
#6884=CARTESIAN_POINT('Ctrl Pts',(0.7960503183159,26.3879210565933,-1.15698088816279));
#6885=CARTESIAN_POINT('Ctrl Pts',(1.10606241295738,26.5962543899266,-0.943679848235541));
#6886=CARTESIAN_POINT('Ctrl Pts',(1.26789024243363,26.80458772326,-0.603949681684177));
#6887=CARTESIAN_POINT('Ctrl Pts',(1.42971807190996,27.0129210565933,-0.264219515132761));
#6888=CARTESIAN_POINT('Ctrl Pts',(1.4,27.2212543899266,0.110909354270855));
#6889=CARTESIAN_POINT('Ctrl Pts',(1.37028192809007,27.42958772326,0.486038223674393));
#6890=CARTESIAN_POINT('Ctrl Pts',(1.15698088816278,27.6379210565933,0.796050318315892));
#6891=CARTESIAN_POINT('Ctrl Pts',(0.943679848235495,27.8462543899266,1.10606241295729));
#6892=CARTESIAN_POINT('Ctrl Pts',(0.603949681684099,28.0545877232599,1.26789024243361));
#6893=CARTESIAN_POINT('Ctrl Pts',(0.264219515132724,28.2629210565933,1.42971807190986));
#6894=CARTESIAN_POINT('Ctrl Pts',(-0.110909354270889,28.4712543899266,1.39999999999997));
#6895=CARTESIAN_POINT('Ctrl Pts',(-0.48603822367442,28.67958772326,1.37028192808997));
#6896=CARTESIAN_POINT('Ctrl Pts',(-0.796050318315921,28.8879210565933,1.15698088816275));
#6897=CARTESIAN_POINT('Ctrl Pts',(-1.10606241295734,29.0962543899266,0.943679848235406));
#6898=CARTESIAN_POINT('Ctrl Pts',(-1.26789024243365,29.30458772326,0.603949681684083));
#6899=CARTESIAN_POINT('Ctrl Pts',(-1.42971807190992,29.5129210565933,0.264219515132621));
#6900=CARTESIAN_POINT('Ctrl Pts',(-1.40000000000002,29.7212543899266,-0.110909354270923));
#6901=CARTESIAN_POINT('Ctrl Pts',(-1.37028192809006,29.92958772326,-0.486038223674506));
#6902=CARTESIAN_POINT('Ctrl Pts',(-1.1569808881628,30.1379210565933,-0.796050318315996));
#6903=CARTESIAN_POINT('Ctrl Pts',(-0.943679848235495,30.3462543899266,-1.10606241295744));
#6904=CARTESIAN_POINT('Ctrl Pts',(-0.60394968168412,30.5545877232599,-1.26789024243366));
#6905=CARTESIAN_POINT('Ctrl Pts',(-0.264219515132702,30.7629210565933,-1.42971807191004));
#6906=CARTESIAN_POINT('Ctrl Pts',(0.110909354270868,30.9712543899266,-1.40000000000007));
#6907=CARTESIAN_POINT('Ctrl Pts',(0.486038223674439,31.17958772326,-1.37028192809015));
#6908=CARTESIAN_POINT('Ctrl Pts',(0.796050318315879,31.3879210565933,-1.15698088816279));
#6909=CARTESIAN_POINT('Ctrl Pts',(1.10606241295736,31.5962543899266,-0.943679848235557));
#6910=CARTESIAN_POINT('Ctrl Pts',(1.26789024243365,31.80458772326,-0.603949681684177));
#6911=CARTESIAN_POINT('Ctrl Pts',(1.42971807190996,32.0129210565933,-0.264219515132783));
#6912=CARTESIAN_POINT('Ctrl Pts',(1.39999999999998,32.2212543899266,0.11090935427085));
#6913=CARTESIAN_POINT('Ctrl Pts',(1.37028192809008,32.42958772326,0.486038223674377));
#6914=CARTESIAN_POINT('Ctrl Pts',(1.15698088816278,32.6379210565933,0.796050318315892));
#6915=CARTESIAN_POINT('Ctrl Pts',(0.943679848235498,32.8462543899267,1.1060624129573));
#6916=CARTESIAN_POINT('Ctrl Pts',(0.603949681684078,33.05458772326,1.26789024243359));
#6917=CARTESIAN_POINT('Ctrl Pts',(0.264219515132705,33.2629210565933,1.4297180719099));
#6918=CARTESIAN_POINT('Ctrl Pts',(-0.110909354270871,33.4712543899267,1.39999999999998));
#6919=CARTESIAN_POINT('Ctrl Pts',(-0.486038223674439,33.67958772326,1.37028192808999));
#6920=CARTESIAN_POINT('Ctrl Pts',(-0.796050318315921,33.8879210565933,1.15698088816275));
#6921=CARTESIAN_POINT('Ctrl Pts',(-1.10606241295736,34.0962543899266,0.943679848235417));
#6922=CARTESIAN_POINT('Ctrl Pts',(-1.26789024243367,34.30458772326,0.603949681684083));
#6923=CARTESIAN_POINT('Ctrl Pts',(-1.42971807190994,34.5129210565933,0.264219515132643));
#6924=CARTESIAN_POINT('Ctrl Pts',(-1.4,34.7212543899266,-0.110909354270923));
#6925=CARTESIAN_POINT('Ctrl Pts',(-1.37028192809004,34.92958772326,-0.486038223674517));
#6926=CARTESIAN_POINT('Ctrl Pts',(-1.1569808881628,35.1379210565933,-0.796050318315944));
#6927=CARTESIAN_POINT('Ctrl Pts',(-0.943679848235495,35.3462543899267,-1.10606241295742));
#6928=CARTESIAN_POINT('Ctrl Pts',(-0.60394968168412,35.55458772326,-1.26789024243366));
#6929=CARTESIAN_POINT('Ctrl Pts',(-0.26421951513268,35.7629210565933,-1.42971807191003));
#6930=CARTESIAN_POINT('Ctrl Pts',(0.110909354270847,35.9712543899266,-1.40000000000004));
#6931=CARTESIAN_POINT('Ctrl Pts',(0.486038223674442,36.17958772326,-1.37028192809012));
#6932=CARTESIAN_POINT('Ctrl Pts',(0.796050318315903,36.3879210565933,-1.15698088816279));
#6933=CARTESIAN_POINT('Ctrl Pts',(1.10606241295738,36.5962543899266,-0.943679848235568));
#6934=CARTESIAN_POINT('Ctrl Pts',(1.26789024243365,36.80458772326,-0.603949681684162));
#6935=CARTESIAN_POINT('Ctrl Pts',(1.42971807190994,37.0129210565933,-0.264219515132788));
#6936=CARTESIAN_POINT('Ctrl Pts',(1.4,37.2212543899267,0.110909354270845));
#6937=CARTESIAN_POINT('Ctrl Pts',(1.37028192809007,37.42958772326,0.486038223674372));
#6938=CARTESIAN_POINT('Ctrl Pts',(1.15698088816278,37.6379210565933,0.796050318315845));
#6939=CARTESIAN_POINT('Ctrl Pts',(0.943679848235495,37.8462543899266,1.1060624129573));
#6940=CARTESIAN_POINT('Ctrl Pts',(0.603949681684099,38.05458772326,1.26789024243359));
#6941=CARTESIAN_POINT('Ctrl Pts',(0.264219515132702,38.2629210565934,1.42971807190987));
#6942=CARTESIAN_POINT('Ctrl Pts',(-0.110909354270891,38.4712543899267,1.39999999999999));
#6943=CARTESIAN_POINT('Ctrl Pts',(-0.486038223674442,38.67958772326,1.37028192808997));
#6944=CARTESIAN_POINT('Ctrl Pts',(-0.796050318315942,38.8879210565933,1.15698088816275));
#6945=CARTESIAN_POINT('Ctrl Pts',(-1.10606241295734,39.0962543899267,0.943679848235401));
#6946=CARTESIAN_POINT('Ctrl Pts',(-1.26789024243367,39.30458772326,0.603949681684089));
#6947=CARTESIAN_POINT('Ctrl Pts',(-1.42971807190992,39.5129210565933,0.264219515132632));
#6948=CARTESIAN_POINT('Ctrl Pts',(-1.40000000000002,39.7212543899266,-0.110909354270923));
#6949=CARTESIAN_POINT('Ctrl Pts',(-2.,-0.27874561007344,-0.110909354270924));
#6950=CARTESIAN_POINT('Ctrl Pts',(-1.97028192809006,-0.0704122767402082,
-0.646807739133109));
#6951=CARTESIAN_POINT('Ctrl Pts',(-1.67659613043344,0.137921056593222,-1.0960503183159));
#6952=CARTESIAN_POINT('Ctrl Pts',(-1.38291033277682,0.346254389926512,-1.54529289749873));
#6953=CARTESIAN_POINT('Ctrl Pts',(-0.903949681684104,0.554587723259871,
-1.78750548470438));
#6954=CARTESIAN_POINT('Ctrl Pts',(-0.424989030591367,0.762921056593226,
-2.02971807190993));
#6955=CARTESIAN_POINT('Ctrl Pts',(0.110909354270878,0.971254389926561,-2.00000000000006));
#6956=CARTESIAN_POINT('Ctrl Pts',(0.646807739133123,1.17958772325984,-1.97028192809007));
#6957=CARTESIAN_POINT('Ctrl Pts',(1.09605031831591,1.38792105659322,-1.67659613043344));
#6958=CARTESIAN_POINT('Ctrl Pts',(1.54529289749868,1.59625438992652,-1.38291033277687));
#6959=CARTESIAN_POINT('Ctrl Pts',(1.78750548470428,1.80458772325989,-0.903949681684113));
#6960=CARTESIAN_POINT('Ctrl Pts',(2.02971807190996,2.01292105659317,-0.42498903059139));
#6961=CARTESIAN_POINT('Ctrl Pts',(2.,2.22125438992656,0.110909354270855));
#6962=CARTESIAN_POINT('Ctrl Pts',(1.97028192809007,2.42958772325984,0.646807739133102));
#6963=CARTESIAN_POINT('Ctrl Pts',(1.67659613043345,2.63792105659317,1.09605031831587));
#6964=CARTESIAN_POINT('Ctrl Pts',(1.38291033277682,2.8462543899265,1.54529289749866));
#6965=CARTESIAN_POINT('Ctrl Pts',(0.903949681684104,3.0545877232599,1.78750548470426));
#6966=CARTESIAN_POINT('Ctrl Pts',(0.424989030591383,3.26292105659317,2.02971807190993));
#6967=CARTESIAN_POINT('Ctrl Pts',(-0.11090935427085,3.47125438992654,1.99999999999995));
#6968=CARTESIAN_POINT('Ctrl Pts',(-0.646807739133109,3.67958772325983,1.97028192809007));
#6969=CARTESIAN_POINT('Ctrl Pts',(-1.0960503183159,3.88792105659323,1.67659613043343));
#6970=CARTESIAN_POINT('Ctrl Pts',(-1.54529289749868,4.09625438992648,1.38291033277681));
#6971=CARTESIAN_POINT('Ctrl Pts',(-1.78750548470431,4.30458772325989,0.903949681684051));
#6972=CARTESIAN_POINT('Ctrl Pts',(-2.02971807190994,4.51292105659318,0.424989030591333));
#6973=CARTESIAN_POINT('Ctrl Pts',(-2.,4.72125438992654,-0.110909354270966));
#6974=CARTESIAN_POINT('Ctrl Pts',(-1.97028192809006,4.92958772325984,-0.646807739133087));
#6975=CARTESIAN_POINT('Ctrl Pts',(-1.67659613043343,5.13792105659321,-1.09605031831595));
#6976=CARTESIAN_POINT('Ctrl Pts',(-1.38291033277682,5.34625438992653,-1.54529289749872));
#6977=CARTESIAN_POINT('Ctrl Pts',(-0.903949681684091,5.5545877232599,-1.78750548470436));
#6978=CARTESIAN_POINT('Ctrl Pts',(-0.424989030591382,5.76292105659322,-2.02971807190993));
#6979=CARTESIAN_POINT('Ctrl Pts',(0.110909354270865,5.97125438992659,-2.00000000000009));
#6980=CARTESIAN_POINT('Ctrl Pts',(0.64680773913311,6.17958772325983,-1.97028192809005));
#6981=CARTESIAN_POINT('Ctrl Pts',(1.0960503183159,6.38792105659326,-1.67659613043349));
#6982=CARTESIAN_POINT('Ctrl Pts',(1.54529289749868,6.5962543899265,-1.38291033277683));
#6983=CARTESIAN_POINT('Ctrl Pts',(1.7875054847043,6.80458772325989,-0.903949681684162));
#6984=CARTESIAN_POINT('Ctrl Pts',(2.02971807190991,7.01292105659322,-0.424989030591398));
#6985=CARTESIAN_POINT('Ctrl Pts',(2.,7.22125438992656,0.110909354270862));
#6986=CARTESIAN_POINT('Ctrl Pts',(1.97028192809006,7.42958772325989,0.646807739133109));
#6987=CARTESIAN_POINT('Ctrl Pts',(1.67659613043344,7.63792105659322,1.09605031831585));
#6988=CARTESIAN_POINT('Ctrl Pts',(1.38291033277683,7.84625438992656,1.54529289749869));
#6989=CARTESIAN_POINT('Ctrl Pts',(0.903949681684104,8.05458772325989,1.78750548470431));
#6990=CARTESIAN_POINT('Ctrl Pts',(0.424989030591398,8.26292105659318,2.02971807190991));
#6991=CARTESIAN_POINT('Ctrl Pts',(-0.110909354270878,8.47125438992655,1.99999999999995));
#6992=CARTESIAN_POINT('Ctrl Pts',(-0.646807739133123,8.67958772325983,1.97028192809004));
#6993=CARTESIAN_POINT('Ctrl Pts',(-1.0960503183159,8.88792105659324,1.67659613043339));
#6994=CARTESIAN_POINT('Ctrl Pts',(-1.54529289749868,9.0962543899265,1.38291033277682));
#6995=CARTESIAN_POINT('Ctrl Pts',(-1.78750548470431,9.3045877232599,0.903949681684085));
#6996=CARTESIAN_POINT('Ctrl Pts',(-2.02971807190993,9.51292105659317,0.424989030591355));
#6997=CARTESIAN_POINT('Ctrl Pts',(-2.,9.72125438992657,-0.110909354270924));
#6998=CARTESIAN_POINT('Ctrl Pts',(-1.97028192809007,9.92958772325983,-0.646807739133123));
#6999=CARTESIAN_POINT('Ctrl Pts',(-1.67659613043344,10.1379210565932,-1.09605031831599));
#7000=CARTESIAN_POINT('Ctrl Pts',(-1.38291033277681,10.3462543899265,-1.54529289749875));
#7001=CARTESIAN_POINT('Ctrl Pts',(-0.903949681684116,10.5545877232599,-1.78750548470438));
#7002=CARTESIAN_POINT('Ctrl Pts',(-0.424989030591382,10.7629210565932,-2.02971807190998));
#7003=CARTESIAN_POINT('Ctrl Pts',(0.110909354270878,10.9712543899266,-2.00000000000009));
#7004=CARTESIAN_POINT('Ctrl Pts',(0.646807739133123,11.1795877232599,-1.97028192809007));
#7005=CARTESIAN_POINT('Ctrl Pts',(1.09605031831591,11.3879210565932,-1.67659613043351));
#7006=CARTESIAN_POINT('Ctrl Pts',(1.54529289749868,11.5962543899265,-1.38291033277682));
#7007=CARTESIAN_POINT('Ctrl Pts',(1.78750548470431,11.8045877232599,-0.903949681684182));
#7008=CARTESIAN_POINT('Ctrl Pts',(2.02971807190993,12.0129210565932,-0.424989030591383));
#7009=CARTESIAN_POINT('Ctrl Pts',(2.,12.2212543899266,0.110909354270862));
#7010=CARTESIAN_POINT('Ctrl Pts',(1.97028192809007,12.4295877232599,0.646807739133051));
#7011=CARTESIAN_POINT('Ctrl Pts',(1.67659613043345,12.6379210565932,1.09605031831589));
#7012=CARTESIAN_POINT('Ctrl Pts',(1.38291033277683,12.8462543899266,1.54529289749867));
#7013=CARTESIAN_POINT('Ctrl Pts',(0.903949681684118,13.0545877232599,1.78750548470425));
#7014=CARTESIAN_POINT('Ctrl Pts',(0.424989030591382,13.2629210565932,2.02971807190993));
#7015=CARTESIAN_POINT('Ctrl Pts',(-0.110909354270864,13.4712543899266,1.99999999999997));
#7016=CARTESIAN_POINT('Ctrl Pts',(-0.646807739133109,13.6795877232599,1.97028192809006));
#7017=CARTESIAN_POINT('Ctrl Pts',(-1.0960503183159,13.8879210565932,1.67659613043339));
#7018=CARTESIAN_POINT('Ctrl Pts',(-1.54529289749868,14.0962543899266,1.38291033277682));
#7019=CARTESIAN_POINT('Ctrl Pts',(-1.7875054847043,14.3045877232599,0.903949681684092));
#7020=CARTESIAN_POINT('Ctrl Pts',(-2.02971807190993,14.5129210565932,0.424989030591326));
#7021=CARTESIAN_POINT('Ctrl Pts',(-2.,14.7212543899266,-0.110909354270938));
#7022=CARTESIAN_POINT('Ctrl Pts',(-1.97028192809006,14.9295877232599,-0.646807739133109));
#7023=CARTESIAN_POINT('Ctrl Pts',(-1.67659613043344,15.1379210565933,-1.09605031831595));
#7024=CARTESIAN_POINT('Ctrl Pts',(-1.38291033277683,15.3462543899265,-1.54529289749874));
#7025=CARTESIAN_POINT('Ctrl Pts',(-0.903949681684104,15.5545877232599,-1.78750548470439));
#7026=CARTESIAN_POINT('Ctrl Pts',(-0.424989030591382,15.7629210565932,-2.02971807190993));
#7027=CARTESIAN_POINT('Ctrl Pts',(0.110909354270852,15.9712543899266,-2.00000000000006));
#7028=CARTESIAN_POINT('Ctrl Pts',(0.646807739133109,16.1795877232599,-1.97028192809006));
#7029=CARTESIAN_POINT('Ctrl Pts',(1.0960503183159,16.3879210565933,-1.67659613043349));
#7030=CARTESIAN_POINT('Ctrl Pts',(1.5452928974987,16.5962543899265,-1.38291033277688));
#7031=CARTESIAN_POINT('Ctrl Pts',(1.78750548470431,16.8045877232599,-0.903949681684148));
#7032=CARTESIAN_POINT('Ctrl Pts',(2.02971807190993,17.0129210565932,-0.424989030591383));
#7033=CARTESIAN_POINT('Ctrl Pts',(2.,17.2212543899266,0.110909354270813));
#7034=CARTESIAN_POINT('Ctrl Pts',(1.97028192809007,17.4295877232599,0.646807739133109));
#7035=CARTESIAN_POINT('Ctrl Pts',(1.67659613043345,17.6379210565933,1.09605031831585));
#7036=CARTESIAN_POINT('Ctrl Pts',(1.38291033277684,17.8462543899265,1.54529289749865));
#7037=CARTESIAN_POINT('Ctrl Pts',(0.903949681684104,18.0545877232599,1.78750548470431));
#7038=CARTESIAN_POINT('Ctrl Pts',(0.424989030591369,18.2629210565932,2.02971807190994));
#7039=CARTESIAN_POINT('Ctrl Pts',(-0.110909354270865,18.4712543899266,2.));
#7040=CARTESIAN_POINT('Ctrl Pts',(-0.646807739133109,18.6795877232599,1.97028192809006));
#7041=CARTESIAN_POINT('Ctrl Pts',(-1.0960503183159,18.8879210565933,1.6765961304334));
#7042=CARTESIAN_POINT('Ctrl Pts',(-1.54529289749867,19.0962543899266,1.38291033277682));
#7043=CARTESIAN_POINT('Ctrl Pts',(-1.78750548470431,19.3045877232599,0.903949681684071));
#7044=CARTESIAN_POINT('Ctrl Pts',(-2.02971807190993,19.5129210565932,0.42498903059134));
#7045=CARTESIAN_POINT('Ctrl Pts',(-2.,19.7212543899266,-0.110909354270924));
#7046=CARTESIAN_POINT('Ctrl Pts',(-1.97028192809006,19.9295877232599,-0.646807739133152));
#7047=CARTESIAN_POINT('Ctrl Pts',(-1.67659613043345,20.1379210565933,-1.09605031831597));
#7048=CARTESIAN_POINT('Ctrl Pts',(-1.38291033277682,20.3462543899266,-1.54529289749875));
#7049=CARTESIAN_POINT('Ctrl Pts',(-0.903949681684103,20.5545877232599,-1.78750548470438));
#7050=CARTESIAN_POINT('Ctrl Pts',(-0.424989030591367,20.7629210565932,-2.02971807190997));
#7051=CARTESIAN_POINT('Ctrl Pts',(0.110909354270864,20.9712543899266,-2.0000000000001));
#7052=CARTESIAN_POINT('Ctrl Pts',(0.64680773913311,21.1795877232599,-1.97028192809011));
#7053=CARTESIAN_POINT('Ctrl Pts',(1.0960503183159,21.3879210565933,-1.67659613043352));
#7054=CARTESIAN_POINT('Ctrl Pts',(1.54529289749868,21.5962543899266,-1.38291033277682));
#7055=CARTESIAN_POINT('Ctrl Pts',(1.78750548470431,21.8045877232599,-0.90394968168419));
#7056=CARTESIAN_POINT('Ctrl Pts',(2.02971807190991,22.0129210565932,-0.42498903059139));
#7057=CARTESIAN_POINT('Ctrl Pts',(2.,22.2212543899266,0.110909354270855));
#7058=CARTESIAN_POINT('Ctrl Pts',(1.9702819280901,22.4295877232599,0.646807739133087));
#7059=CARTESIAN_POINT('Ctrl Pts',(1.67659613043345,22.6379210565933,1.09605031831588));
#7060=CARTESIAN_POINT('Ctrl Pts',(1.38291033277683,22.8462543899266,1.54529289749862));
#7061=CARTESIAN_POINT('Ctrl Pts',(0.903949681684118,23.0545877232599,1.78750548470426));
#7062=CARTESIAN_POINT('Ctrl Pts',(0.424989030591383,23.2629210565932,2.02971807190993));
#7063=CARTESIAN_POINT('Ctrl Pts',(-0.110909354270864,23.4712543899266,1.99999999999997));
#7064=CARTESIAN_POINT('Ctrl Pts',(-0.646807739133109,23.6795877232599,1.97028192809003));
#7065=CARTESIAN_POINT('Ctrl Pts',(-1.09605031831588,23.8879210565933,1.67659613043339));
#7066=CARTESIAN_POINT('Ctrl Pts',(-1.54529289749869,24.0962543899266,1.38291033277682));
#7067=CARTESIAN_POINT('Ctrl Pts',(-1.78750548470431,24.3045877232599,0.903949681684092));
#7068=CARTESIAN_POINT('Ctrl Pts',(-2.02971807190995,24.5129210565932,0.424989030591319));
#7069=CARTESIAN_POINT('Ctrl Pts',(-2.,24.7212543899266,-0.110909354270938));
#7070=CARTESIAN_POINT('Ctrl Pts',(-1.97028192809005,24.9295877232599,-0.646807739133109));
#7071=CARTESIAN_POINT('Ctrl Pts',(-1.67659613043344,25.1379210565933,-1.09605031831594));
#7072=CARTESIAN_POINT('Ctrl Pts',(-1.38291033277682,25.3462543899266,-1.54529289749872));
#7073=CARTESIAN_POINT('Ctrl Pts',(-0.903949681684104,25.55458772326,-1.7875054847044));
#7074=CARTESIAN_POINT('Ctrl Pts',(-0.424989030591382,25.7629210565933,-2.02971807190993));
#7075=CARTESIAN_POINT('Ctrl Pts',(0.110909354270864,25.9712543899266,-2.00000000000006));
#7076=CARTESIAN_POINT('Ctrl Pts',(0.646807739133109,26.1795877232599,-1.97028192809006));
#7077=CARTESIAN_POINT('Ctrl Pts',(1.0960503183159,26.3879210565933,-1.67659613043348));
#7078=CARTESIAN_POINT('Ctrl Pts',(1.5452928974987,26.5962543899266,-1.38291033277687));
#7079=CARTESIAN_POINT('Ctrl Pts',(1.78750548470431,26.80458772326,-0.903949681684155));
#7080=CARTESIAN_POINT('Ctrl Pts',(2.02971807190993,27.0129210565933,-0.424989030591383));
#7081=CARTESIAN_POINT('Ctrl Pts',(2.00000000000003,27.2212543899266,0.11090935427082));
#7082=CARTESIAN_POINT('Ctrl Pts',(1.97028192809007,27.4295877232599,0.646807739133109));
#7083=CARTESIAN_POINT('Ctrl Pts',(1.67659613043345,27.6379210565933,1.09605031831587));
#7084=CARTESIAN_POINT('Ctrl Pts',(1.38291033277684,27.8462543899266,1.54529289749868));
#7085=CARTESIAN_POINT('Ctrl Pts',(0.903949681684103,28.0545877232599,1.78750548470431));
#7086=CARTESIAN_POINT('Ctrl Pts',(0.424989030591382,28.2629210565932,2.02971807190993));
#7087=CARTESIAN_POINT('Ctrl Pts',(-0.110909354270852,28.4712543899266,1.99999999999998));
#7088=CARTESIAN_POINT('Ctrl Pts',(-0.646807739133109,28.6795877232599,1.97028192809006));
#7089=CARTESIAN_POINT('Ctrl Pts',(-1.0960503183159,28.8879210565933,1.67659613043341));
#7090=CARTESIAN_POINT('Ctrl Pts',(-1.54529289749868,29.0962543899266,1.38291033277682));
#7091=CARTESIAN_POINT('Ctrl Pts',(-1.78750548470432,29.30458772326,0.903949681684071));
#7092=CARTESIAN_POINT('Ctrl Pts',(-2.02971807190993,29.5129210565933,0.42498903059134));
#7093=CARTESIAN_POINT('Ctrl Pts',(-2.,29.7212543899266,-0.110909354270917));
#7094=CARTESIAN_POINT('Ctrl Pts',(-1.97028192809006,29.9295877232599,-0.646807739133087));
#7095=CARTESIAN_POINT('Ctrl Pts',(-1.67659613043345,30.1379210565933,-1.09605031831597));
#7096=CARTESIAN_POINT('Ctrl Pts',(-1.38291033277683,30.3462543899266,-1.54529289749872));
#7097=CARTESIAN_POINT('Ctrl Pts',(-0.903949681684103,30.55458772326,-1.78750548470437));
#7098=CARTESIAN_POINT('Ctrl Pts',(-0.424989030591367,30.7629210565933,-2.02971807190996));
#7099=CARTESIAN_POINT('Ctrl Pts',(0.110909354270865,30.9712543899266,-2.00000000000009));
#7100=CARTESIAN_POINT('Ctrl Pts',(0.646807739133123,31.1795877232599,-1.97028192809004));
#7101=CARTESIAN_POINT('Ctrl Pts',(1.0960503183159,31.3879210565933,-1.67659613043352));
#7102=CARTESIAN_POINT('Ctrl Pts',(1.54529289749868,31.5962543899266,-1.38291033277685));
#7103=CARTESIAN_POINT('Ctrl Pts',(1.78750548470431,31.80458772326,-0.903949681684169));
#7104=CARTESIAN_POINT('Ctrl Pts',(2.02971807190993,32.0129210565933,-0.424989030591419));
#7105=CARTESIAN_POINT('Ctrl Pts',(2.,32.2212543899266,0.110909354270869));
#7106=CARTESIAN_POINT('Ctrl Pts',(1.97028192809004,32.4295877232599,0.646807739133087));
#7107=CARTESIAN_POINT('Ctrl Pts',(1.67659613043345,32.6379210565933,1.09605031831587));
#7108=CARTESIAN_POINT('Ctrl Pts',(1.38291033277682,32.8462543899266,1.54529289749868));
#7109=CARTESIAN_POINT('Ctrl Pts',(0.903949681684104,33.0545877232599,1.78750548470431));
#7110=CARTESIAN_POINT('Ctrl Pts',(0.424989030591383,33.2629210565932,2.02971807190993));
#7111=CARTESIAN_POINT('Ctrl Pts',(-0.110909354270864,33.4712543899267,1.99999999999997));
#7112=CARTESIAN_POINT('Ctrl Pts',(-0.646807739133109,33.6795877232599,1.97028192809004));
#7113=CARTESIAN_POINT('Ctrl Pts',(-1.09605031831588,33.8879210565934,1.6765961304334));
#7114=CARTESIAN_POINT('Ctrl Pts',(-1.54529289749868,34.0962543899266,1.38291033277683));
#7115=CARTESIAN_POINT('Ctrl Pts',(-1.78750548470431,34.30458772326,0.903949681684037));
#7116=CARTESIAN_POINT('Ctrl Pts',(-2.02971807190994,34.5129210565932,0.424989030591383));
#7117=CARTESIAN_POINT('Ctrl Pts',(-2.,34.7212543899267,-0.110909354270938));
#7118=CARTESIAN_POINT('Ctrl Pts',(-1.97028192809006,34.9295877232599,-0.646807739133123));
#7119=CARTESIAN_POINT('Ctrl Pts',(-1.67659613043344,35.1379210565933,-1.09605031831594));
#7120=CARTESIAN_POINT('Ctrl Pts',(-1.38291033277682,35.3462543899267,-1.54529289749875));
#7121=CARTESIAN_POINT('Ctrl Pts',(-0.903949681684103,35.55458772326,-1.78750548470439));
#7122=CARTESIAN_POINT('Ctrl Pts',(-0.424989030591382,35.7629210565932,-2.02971807190993));
#7123=CARTESIAN_POINT('Ctrl Pts',(0.110909354270864,35.9712543899267,-2.00000000000003));
#7124=CARTESIAN_POINT('Ctrl Pts',(0.64680773913311,36.1795877232599,-1.97028192809006));
#7125=CARTESIAN_POINT('Ctrl Pts',(1.0960503183159,36.3879210565933,-1.67659613043348));
#7126=CARTESIAN_POINT('Ctrl Pts',(1.54529289749869,36.5962543899266,-1.38291033277682));
#7127=CARTESIAN_POINT('Ctrl Pts',(1.78750548470431,36.80458772326,-0.903949681684127));
#7128=CARTESIAN_POINT('Ctrl Pts',(2.02971807190993,37.0129210565932,-0.424989030591383));
#7129=CARTESIAN_POINT('Ctrl Pts',(2.,37.2212543899267,0.110909354270834));
#7130=CARTESIAN_POINT('Ctrl Pts',(1.97028192809006,37.4295877232599,0.646807739133109));
#7131=CARTESIAN_POINT('Ctrl Pts',(1.67659613043345,37.6379210565933,1.09605031831588));
#7132=CARTESIAN_POINT('Ctrl Pts',(1.38291033277681,37.8462543899266,1.54529289749865));
#7133=CARTESIAN_POINT('Ctrl Pts',(0.903949681684104,38.0545877232599,1.78750548470431));
#7134=CARTESIAN_POINT('Ctrl Pts',(0.424989030591383,38.2629210565933,2.02971807190991));
#7135=CARTESIAN_POINT('Ctrl Pts',(-0.11090935427085,38.4712543899266,1.99999999999995));
#7136=CARTESIAN_POINT('Ctrl Pts',(-0.64680773913311,38.67958772326,1.97028192809006));
#7137=CARTESIAN_POINT('Ctrl Pts',(-1.0960503183159,38.8879210565933,1.67659613043344));
#7138=CARTESIAN_POINT('Ctrl Pts',(-1.54529289749868,39.0962543899266,1.38291033277682));
#7139=CARTESIAN_POINT('Ctrl Pts',(-1.78750548470431,39.30458772326,0.903949681684064));
#7140=CARTESIAN_POINT('Ctrl Pts',(-2.02971807190993,39.5129210565932,0.424989030591369));
#7141=CARTESIAN_POINT('Ctrl Pts',(-2.,39.7212543899267,-0.110909354270917));
#7142=CARTESIAN_POINT('Ctrl Pts',(-2.59980895670905,-0.278745610073447,
-0.11090935427086));
#7143=CARTESIAN_POINT('Ctrl Pts',(-2.5700908847991,-0.0704122767401095,
-0.807526064696338));
#7144=CARTESIAN_POINT('Ctrl Pts',(-2.19604592436092,0.137921056593207,-1.39595479667049));
#7145=CARTESIAN_POINT('Ctrl Pts',(-1.82200096392271,0.346254389926554,-1.98438352864466));
#7146=CARTESIAN_POINT('Ctrl Pts',(-1.20385416003863,0.554587723259855,-2.30695527863182));
#7147=CARTESIAN_POINT('Ctrl Pts',(-0.585707356154528,0.762921056593228,
-2.62952702861907));
#7148=CARTESIAN_POINT('Ctrl Pts',(0.11090935427086,0.971254389926535,-2.59980895670912));
#7149=CARTESIAN_POINT('Ctrl Pts',(0.807526064696268,1.17958772325987,-2.57009088479919));
#7150=CARTESIAN_POINT('Ctrl Pts',(1.39595479667041,1.38792105659322,-2.196045924361));
#7151=CARTESIAN_POINT('Ctrl Pts',(1.98438352864458,1.59625438992655,-1.82200096392273));
#7152=CARTESIAN_POINT('Ctrl Pts',(2.30695527863176,1.80458772325989,-1.20385416003868));
#7153=CARTESIAN_POINT('Ctrl Pts',(2.62952702861898,2.01292105659322,-0.58570735615462));
#7154=CARTESIAN_POINT('Ctrl Pts',(2.59980895670903,2.22125438992652,0.110909354270808));
#7155=CARTESIAN_POINT('Ctrl Pts',(2.57009088479911,2.42958772325989,0.807526064696155));
#7156=CARTESIAN_POINT('Ctrl Pts',(2.1960459243609,2.63792105659321,1.39595479667038));
#7157=CARTESIAN_POINT('Ctrl Pts',(1.82200096392273,2.84625438992655,1.98438352864455));
#7158=CARTESIAN_POINT('Ctrl Pts',(1.20385416003861,3.05458772325989,2.3069552786317));
#7159=CARTESIAN_POINT('Ctrl Pts',(0.585707356154531,3.26292105659321,2.62952702861891));
#7160=CARTESIAN_POINT('Ctrl Pts',(-0.11090935427086,3.47125438992654,2.59980895670896));
#7161=CARTESIAN_POINT('Ctrl Pts',(-0.807526064696246,3.67958772325991,2.57009088479904));
#7162=CARTESIAN_POINT('Ctrl Pts',(-1.39595479667041,3.8879210565932,2.1960459243609));
#7163=CARTESIAN_POINT('Ctrl Pts',(-1.98438352864456,4.09625438992658,1.82200096392269));
#7164=CARTESIAN_POINT('Ctrl Pts',(-2.3069552786318,4.30458772325988,1.20385416003854));
#7165=CARTESIAN_POINT('Ctrl Pts',(-2.62952702861897,4.51292105659321,0.585707356154447));
#7166=CARTESIAN_POINT('Ctrl Pts',(-2.59980895670904,4.72125438992652,-0.110909354270855));
#7167=CARTESIAN_POINT('Ctrl Pts',(-2.5700908847991,4.92958772325988,-0.807526064696333));
#7168=CARTESIAN_POINT('Ctrl Pts',(-2.19604592436094,5.13792105659322,-1.39595479667042));
#7169=CARTESIAN_POINT('Ctrl Pts',(-1.82200096392273,5.34625438992655,-1.98438352864466));
#7170=CARTESIAN_POINT('Ctrl Pts',(-1.20385416003865,5.55458772325989,-2.30695527863179));
#7171=CARTESIAN_POINT('Ctrl Pts',(-0.585707356154528,5.76292105659322,-2.62952702861911));
#7172=CARTESIAN_POINT('Ctrl Pts',(0.110909354270839,5.97125438992656,-2.59980895670905));
#7173=CARTESIAN_POINT('Ctrl Pts',(0.807526064696268,6.1795877232599,-2.57009088479919));
#7174=CARTESIAN_POINT('Ctrl Pts',(1.39595479667041,6.38792105659324,-2.196045924361));
#7175=CARTESIAN_POINT('Ctrl Pts',(1.9843835286446,6.59625438992657,-1.82200096392282));
#7176=CARTESIAN_POINT('Ctrl Pts',(2.30695527863178,6.80458772325989,-1.20385416003871));
#7177=CARTESIAN_POINT('Ctrl Pts',(2.62952702861898,7.01292105659322,-0.585707356154609));
#7178=CARTESIAN_POINT('Ctrl Pts',(2.59980895670904,7.22125438992658,0.110909354270855));
#7179=CARTESIAN_POINT('Ctrl Pts',(2.57009088479913,7.42958772325989,0.807526064696236));
#7180=CARTESIAN_POINT('Ctrl Pts',(2.19604592436092,7.63792105659324,1.39595479667033));
#7181=CARTESIAN_POINT('Ctrl Pts',(1.82200096392274,7.84625438992655,1.98438352864452));
#7182=CARTESIAN_POINT('Ctrl Pts',(1.20385416003861,8.05458772325989,2.30695527863176));
#7183=CARTESIAN_POINT('Ctrl Pts',(0.585707356154531,8.26292105659324,2.62952702861887));
#7184=CARTESIAN_POINT('Ctrl Pts',(-0.11090935427086,8.47125438992656,2.59980895670904));
#7185=CARTESIAN_POINT('Ctrl Pts',(-0.807526064696241,8.67958772325989,2.57009088479907));
#7186=CARTESIAN_POINT('Ctrl Pts',(-1.39595479667041,8.88792105659322,2.19604592436091));
#7187=CARTESIAN_POINT('Ctrl Pts',(-1.98438352864456,9.09625438992657,1.82200096392265));
#7188=CARTESIAN_POINT('Ctrl Pts',(-2.3069552786318,9.30458772325988,1.20385416003854));
#7189=CARTESIAN_POINT('Ctrl Pts',(-2.62952702861897,9.51292105659323,0.585707356154528));
#7190=CARTESIAN_POINT('Ctrl Pts',(-2.59980895670904,9.72125438992655,-0.11090935427086));
#7191=CARTESIAN_POINT('Ctrl Pts',(-2.57009088479911,9.92958772325989,-0.807526064696419));
#7192=CARTESIAN_POINT('Ctrl Pts',(-2.19604592436092,10.1379210565932,-1.39595479667049));
#7193=CARTESIAN_POINT('Ctrl Pts',(-1.82200096392273,10.3462543899266,-1.98438352864459));
#7194=CARTESIAN_POINT('Ctrl Pts',(-1.20385416003865,10.5545877232599,-2.30695527863179));
#7195=CARTESIAN_POINT('Ctrl Pts',(-0.585707356154528,10.7629210565933,-2.6295270286191));
#7196=CARTESIAN_POINT('Ctrl Pts',(0.11090935427086,10.9712543899266,-2.59980895670905));
#7197=CARTESIAN_POINT('Ctrl Pts',(0.807526064696249,11.1795877232599,-2.57009088479919));
#7198=CARTESIAN_POINT('Ctrl Pts',(1.39595479667039,11.3879210565932,-2.196045924361));
#7199=CARTESIAN_POINT('Ctrl Pts',(1.98438352864458,11.5962543899266,-1.82200096392274));
#7200=CARTESIAN_POINT('Ctrl Pts',(2.30695527863176,11.8045877232599,-1.20385416003872));
#7201=CARTESIAN_POINT('Ctrl Pts',(2.62952702861898,12.0129210565933,-0.585707356154631));
#7202=CARTESIAN_POINT('Ctrl Pts',(2.59980895670904,12.2212543899266,0.11090935427085));
#7203=CARTESIAN_POINT('Ctrl Pts',(2.57009088479911,12.4295877232599,0.807526064696171));
#7204=CARTESIAN_POINT('Ctrl Pts',(2.1960459243609,12.6379210565932,1.39595479667034));
#7205=CARTESIAN_POINT('Ctrl Pts',(1.82200096392273,12.8462543899266,1.98438352864456));
#7206=CARTESIAN_POINT('Ctrl Pts',(1.20385416003863,13.0545877232599,2.30695527863174));
#7207=CARTESIAN_POINT('Ctrl Pts',(0.585707356154552,13.2629210565932,2.62952702861889));
#7208=CARTESIAN_POINT('Ctrl Pts',(-0.11090935427086,13.4712543899266,2.599808956709));
#7209=CARTESIAN_POINT('Ctrl Pts',(-0.807526064696246,13.6795877232599,2.57009088479904));
#7210=CARTESIAN_POINT('Ctrl Pts',(-1.39595479667043,13.8879210565933,2.1960459243609));
#7211=CARTESIAN_POINT('Ctrl Pts',(-1.98438352864458,14.0962543899266,1.82200096392269));
#7212=CARTESIAN_POINT('Ctrl Pts',(-2.3069552786318,14.3045877232599,1.20385416003854));
#7213=CARTESIAN_POINT('Ctrl Pts',(-2.62952702861897,14.5129210565932,0.585707356154453));
#7214=CARTESIAN_POINT('Ctrl Pts',(-2.59980895670906,14.7212543899266,-0.110909354270865));
#7215=CARTESIAN_POINT('Ctrl Pts',(-2.57009088479911,14.9295877232599,-0.807526064696338));
#7216=CARTESIAN_POINT('Ctrl Pts',(-2.19604592436092,15.1379210565932,-1.39595479667049));
#7217=CARTESIAN_POINT('Ctrl Pts',(-1.82200096392273,15.3462543899266,-1.98438352864467));
#7218=CARTESIAN_POINT('Ctrl Pts',(-1.20385416003865,15.5545877232599,-2.30695527863179));
#7219=CARTESIAN_POINT('Ctrl Pts',(-0.585707356154509,15.7629210565933,-2.62952702861908));
#7220=CARTESIAN_POINT('Ctrl Pts',(0.110909354270839,15.9712543899266,-2.59980895670905));
#7221=CARTESIAN_POINT('Ctrl Pts',(0.807526064696268,16.1795877232599,-2.57009088479922));
#7222=CARTESIAN_POINT('Ctrl Pts',(1.39595479667041,16.3879210565933,-2.19604592436098));
#7223=CARTESIAN_POINT('Ctrl Pts',(1.9843835286446,16.5962543899266,-1.82200096392274));
#7224=CARTESIAN_POINT('Ctrl Pts',(2.30695527863178,16.8045877232599,-1.20385416003872));
#7225=CARTESIAN_POINT('Ctrl Pts',(2.629527028619,17.0129210565933,-0.58570735615462));
#7226=CARTESIAN_POINT('Ctrl Pts',(2.59980895670902,17.2212543899266,0.110909354270855));
#7227=CARTESIAN_POINT('Ctrl Pts',(2.57009088479911,17.42958772326,0.807526064696182));
#7228=CARTESIAN_POINT('Ctrl Pts',(2.1960459243609,17.6379210565933,1.3959547966704));
#7229=CARTESIAN_POINT('Ctrl Pts',(1.82200096392273,17.8462543899266,1.98438352864452));
#7230=CARTESIAN_POINT('Ctrl Pts',(1.20385416003863,18.0545877232599,2.30695527863173));
#7231=CARTESIAN_POINT('Ctrl Pts',(0.585707356154531,18.2629210565933,2.62952702861889));
#7232=CARTESIAN_POINT('Ctrl Pts',(-0.11090935427086,18.4712543899266,2.599808956709));
#7233=CARTESIAN_POINT('Ctrl Pts',(-0.807526064696244,18.6795877232599,2.57009088479907));
#7234=CARTESIAN_POINT('Ctrl Pts',(-1.39595479667041,18.8879210565933,2.19604592436089));
#7235=CARTESIAN_POINT('Ctrl Pts',(-1.98438352864458,19.0962543899266,1.82200096392266));
#7236=CARTESIAN_POINT('Ctrl Pts',(-2.3069552786318,19.3045877232599,1.20385416003862));
#7237=CARTESIAN_POINT('Ctrl Pts',(-2.62952702861896,19.5129210565933,0.585707356154491));
#7238=CARTESIAN_POINT('Ctrl Pts',(-2.59980895670904,19.7212543899266,-0.110909354270865));
#7239=CARTESIAN_POINT('Ctrl Pts',(-2.5700908847991,19.9295877232599,-0.8075260646963));
#7240=CARTESIAN_POINT('Ctrl Pts',(-2.19604592436092,20.1379210565933,-1.39595479667049));
#7241=CARTESIAN_POINT('Ctrl Pts',(-1.82200096392271,20.3462543899266,-1.98438352864466));
#7242=CARTESIAN_POINT('Ctrl Pts',(-1.20385416003865,20.5545877232599,-2.30695527863182));
#7243=CARTESIAN_POINT('Ctrl Pts',(-0.585707356154528,20.7629210565933,-2.62952702861907));
#7244=CARTESIAN_POINT('Ctrl Pts',(0.110909354270839,20.9712543899266,-2.59980895670905));
#7245=CARTESIAN_POINT('Ctrl Pts',(0.807526064696249,21.1795877232599,-2.5700908847992));
#7246=CARTESIAN_POINT('Ctrl Pts',(1.39595479667039,21.3879210565933,-2.19604592436098));
#7247=CARTESIAN_POINT('Ctrl Pts',(1.9843835286446,21.5962543899266,-1.8220009639228));
#7248=CARTESIAN_POINT('Ctrl Pts',(2.30695527863176,21.8045877232599,-1.20385416003872));
#7249=CARTESIAN_POINT('Ctrl Pts',(2.62952702861898,22.0129210565933,-0.585707356154604));
#7250=CARTESIAN_POINT('Ctrl Pts',(2.59980895670904,22.2212543899266,0.11090935427085));
#7251=CARTESIAN_POINT('Ctrl Pts',(2.57009088479913,22.42958772326,0.807526064696171));
#7252=CARTESIAN_POINT('Ctrl Pts',(2.19604592436092,22.6379210565933,1.3959547966704));
#7253=CARTESIAN_POINT('Ctrl Pts',(1.82200096392275,22.8462543899266,1.98438352864454));
#7254=CARTESIAN_POINT('Ctrl Pts',(1.20385416003863,23.0545877232599,2.30695527863174));
#7255=CARTESIAN_POINT('Ctrl Pts',(0.58570735615455,23.2629210565933,2.62952702861891));
#7256=CARTESIAN_POINT('Ctrl Pts',(-0.110909354270881,23.4712543899266,2.599808956709));
#7257=CARTESIAN_POINT('Ctrl Pts',(-0.807526064696225,23.6795877232599,2.57009088479905));
#7258=CARTESIAN_POINT('Ctrl Pts',(-1.39595479667043,23.8879210565933,2.19604592436087));
#7259=CARTESIAN_POINT('Ctrl Pts',(-1.98438352864458,24.0962543899266,1.82200096392269));
#7260=CARTESIAN_POINT('Ctrl Pts',(-2.3069552786318,24.3045877232599,1.20385416003862));
#7261=CARTESIAN_POINT('Ctrl Pts',(-2.62952702861898,24.5129210565933,0.585707356154485));
#7262=CARTESIAN_POINT('Ctrl Pts',(-2.59980895670906,24.7212543899266,-0.110909354270829));
#7263=CARTESIAN_POINT('Ctrl Pts',(-2.5700908847991,24.92958772326,-0.807526064696322));
#7264=CARTESIAN_POINT('Ctrl Pts',(-2.19604592436094,25.1379210565933,-1.39595479667048));
#7265=CARTESIAN_POINT('Ctrl Pts',(-1.82200096392273,25.3462543899266,-1.98438352864461));
#7266=CARTESIAN_POINT('Ctrl Pts',(-1.20385416003865,25.5545877232599,-2.30695527863182));
#7267=CARTESIAN_POINT('Ctrl Pts',(-0.585707356154509,25.7629210565933,-2.62952702861915));
#7268=CARTESIAN_POINT('Ctrl Pts',(0.110909354270839,25.9712543899266,-2.59980895670905));
#7269=CARTESIAN_POINT('Ctrl Pts',(0.807526064696246,26.17958772326,-2.57009088479919));
#7270=CARTESIAN_POINT('Ctrl Pts',(1.39595479667039,26.3879210565933,-2.19604592436098));
#7271=CARTESIAN_POINT('Ctrl Pts',(1.98438352864458,26.5962543899266,-1.82200096392281));
#7272=CARTESIAN_POINT('Ctrl Pts',(2.30695527863176,26.80458772326,-1.20385416003873));
#7273=CARTESIAN_POINT('Ctrl Pts',(2.629527028619,27.0129210565933,-0.585707356154641));
#7274=CARTESIAN_POINT('Ctrl Pts',(2.59980895670904,27.2212543899266,0.110909354270782));
#7275=CARTESIAN_POINT('Ctrl Pts',(2.57009088479911,27.42958772326,0.807526064696187));
#7276=CARTESIAN_POINT('Ctrl Pts',(2.1960459243609,27.6379210565932,1.39595479667041));
#7277=CARTESIAN_POINT('Ctrl Pts',(1.82200096392273,27.8462543899266,1.98438352864453));
#7278=CARTESIAN_POINT('Ctrl Pts',(1.20385416003861,28.05458772326,2.30695527863173));
#7279=CARTESIAN_POINT('Ctrl Pts',(0.585707356154552,28.2629210565933,2.62952702861888));
#7280=CARTESIAN_POINT('Ctrl Pts',(-0.11090935427086,28.4712543899266,2.59980895670899));
#7281=CARTESIAN_POINT('Ctrl Pts',(-0.807526064696246,28.67958772326,2.57009088479907));
#7282=CARTESIAN_POINT('Ctrl Pts',(-1.39595479667043,28.8879210565933,2.19604592436087));
#7283=CARTESIAN_POINT('Ctrl Pts',(-1.98438352864458,29.0962543899266,1.82200096392266));
#7284=CARTESIAN_POINT('Ctrl Pts',(-2.3069552786318,29.3045877232599,1.20385416003859));
#7285=CARTESIAN_POINT('Ctrl Pts',(-2.62952702861898,29.5129210565933,0.585707356154469));
#7286=CARTESIAN_POINT('Ctrl Pts',(-2.59980895670906,29.7212543899266,-0.110909354270912));
#7287=CARTESIAN_POINT('Ctrl Pts',(-2.5700908847991,29.92958772326,-0.807526064696306));
#7288=CARTESIAN_POINT('Ctrl Pts',(-2.19604592436092,30.1379210565933,-1.39595479667046));
#7289=CARTESIAN_POINT('Ctrl Pts',(-1.82200096392273,30.3462543899266,-1.98438352864468));
#7290=CARTESIAN_POINT('Ctrl Pts',(-1.20385416003865,30.5545877232599,-2.30695527863181));
#7291=CARTESIAN_POINT('Ctrl Pts',(-0.585707356154507,30.7629210565933,-2.6295270286191));
#7292=CARTESIAN_POINT('Ctrl Pts',(0.110909354270839,30.9712543899266,-2.59980895670908));
#7293=CARTESIAN_POINT('Ctrl Pts',(0.807526064696246,31.17958772326,-2.57009088479918));
#7294=CARTESIAN_POINT('Ctrl Pts',(1.39595479667041,31.3879210565933,-2.19604592436097));
#7295=CARTESIAN_POINT('Ctrl Pts',(1.9843835286446,31.5962543899266,-1.82200096392281));
#7296=CARTESIAN_POINT('Ctrl Pts',(2.30695527863178,31.80458772326,-1.20385416003872));
#7297=CARTESIAN_POINT('Ctrl Pts',(2.629527028619,32.0129210565933,-0.585707356154615));
#7298=CARTESIAN_POINT('Ctrl Pts',(2.59980895670902,32.2212543899266,0.110909354270782));
#7299=CARTESIAN_POINT('Ctrl Pts',(2.57009088479913,32.4295877232599,0.807526064696171));
#7300=CARTESIAN_POINT('Ctrl Pts',(2.1960459243609,32.6379210565933,1.3959547966704));
#7301=CARTESIAN_POINT('Ctrl Pts',(1.82200096392275,32.8462543899266,1.98438352864454));
#7302=CARTESIAN_POINT('Ctrl Pts',(1.20385416003863,33.05458772326,2.30695527863173));
#7303=CARTESIAN_POINT('Ctrl Pts',(0.585707356154531,33.2629210565933,2.62952702861892));
#7304=CARTESIAN_POINT('Ctrl Pts',(-0.11090935427086,33.4712543899266,2.59980895670899));
#7305=CARTESIAN_POINT('Ctrl Pts',(-0.807526064696225,33.67958772326,2.57009088479904));
#7306=CARTESIAN_POINT('Ctrl Pts',(-1.39595479667043,33.8879210565933,2.19604592436087));
#7307=CARTESIAN_POINT('Ctrl Pts',(-1.98438352864458,34.0962543899266,1.82200096392268));
#7308=CARTESIAN_POINT('Ctrl Pts',(-2.30695527863178,34.3045877232599,1.2038541600386));
#7309=CARTESIAN_POINT('Ctrl Pts',(-2.62952702861898,34.5129210565933,0.585707356154485));
#7310=CARTESIAN_POINT('Ctrl Pts',(-2.59980895670904,34.7212543899266,-0.110909354270923));
#7311=CARTESIAN_POINT('Ctrl Pts',(-2.5700908847991,34.92958772326,-0.807526064696322));
#7312=CARTESIAN_POINT('Ctrl Pts',(-2.19604592436092,35.1379210565933,-1.39595479667045));
#7313=CARTESIAN_POINT('Ctrl Pts',(-1.82200096392271,35.3462543899266,-1.98438352864466));
#7314=CARTESIAN_POINT('Ctrl Pts',(-1.20385416003863,35.55458772326,-2.30695527863182));
#7315=CARTESIAN_POINT('Ctrl Pts',(-0.585707356154509,35.7629210565933,-2.62952702861903));
#7316=CARTESIAN_POINT('Ctrl Pts',(0.110909354270858,35.9712543899266,-2.59980895670908));
#7317=CARTESIAN_POINT('Ctrl Pts',(0.807526064696268,36.17958772326,-2.57009088479921));
#7318=CARTESIAN_POINT('Ctrl Pts',(1.3959547966704,36.3879210565933,-2.19604592436097));
#7319=CARTESIAN_POINT('Ctrl Pts',(1.98438352864458,36.5962543899266,-1.82200096392283));
#7320=CARTESIAN_POINT('Ctrl Pts',(2.30695527863176,36.80458772326,-1.20385416003864));
#7321=CARTESIAN_POINT('Ctrl Pts',(2.629527028619,37.0129210565933,-0.585707356154631));
#7322=CARTESIAN_POINT('Ctrl Pts',(2.59980895670904,37.2212543899266,0.110909354270793));
#7323=CARTESIAN_POINT('Ctrl Pts',(2.57009088479913,37.42958772326,0.807526064696182));
#7324=CARTESIAN_POINT('Ctrl Pts',(2.1960459243609,37.6379210565933,1.39595479667037));
#7325=CARTESIAN_POINT('Ctrl Pts',(1.82200096392275,37.8462543899266,1.98438352864452));
#7326=CARTESIAN_POINT('Ctrl Pts',(1.20385416003863,38.05458772326,2.30695527863174));
#7327=CARTESIAN_POINT('Ctrl Pts',(0.585707356154552,38.2629210565933,2.62952702861889));
#7328=CARTESIAN_POINT('Ctrl Pts',(-0.110909354270881,38.4712543899266,2.599808956709));
#7329=CARTESIAN_POINT('Ctrl Pts',(-0.807526064696225,38.67958772326,2.57009088479908));
#7330=CARTESIAN_POINT('Ctrl Pts',(-1.39595479667043,38.8879210565933,2.19604592436087));
#7331=CARTESIAN_POINT('Ctrl Pts',(-1.98438352864458,39.0962543899267,1.82200096392266));
#7332=CARTESIAN_POINT('Ctrl Pts',(-2.30695527863182,39.30458772326,1.20385416003859));
#7333=CARTESIAN_POINT('Ctrl Pts',(-2.62952702861897,39.5129210565933,0.585707356154453));
#7334=CARTESIAN_POINT('Ctrl Pts',(-2.59980895670906,39.7212543899267,-0.110909354270912));
#7335=CARTESIAN_POINT('Ctrl Pts',(-2.599999979715,0.278627239826795,0.110862256246242));
#7336=CARTESIAN_POINT('Ctrl Pts',(-2.62970543174724,0.486960573160142,-0.585805638639407));
#7337=CARTESIAN_POINT('Ctrl Pts',(-2.30709716039532,0.695293906493465,-1.20399045962746));
#7338=CARTESIAN_POINT('Ctrl Pts',(-1.98448888904339,0.903627239826795,-1.82217528061545));
#7339=CARTESIAN_POINT('Ctrl Pts',(-1.39600952008762,1.11196057316013,-2.19623490414907));
#7340=CARTESIAN_POINT('Ctrl Pts',(-0.807530151131804,1.32029390649347,-2.57029452768285));
#7341=CARTESIAN_POINT('Ctrl Pts',(-0.110862256246242,1.5286272398268,-2.59999997971506));
#7342=CARTESIAN_POINT('Ctrl Pts',(0.585805638639342,1.73696057316013,-2.62970543174735));
#7343=CARTESIAN_POINT('Ctrl Pts',(1.20399045962738,1.94529390649346,-2.3070971603954));
#7344=CARTESIAN_POINT('Ctrl Pts',(1.82217528061545,2.15362723982677,-1.98448888904346));
#7345=CARTESIAN_POINT('Ctrl Pts',(2.19623490414905,2.36196057316013,-1.3960095200876));
#7346=CARTESIAN_POINT('Ctrl Pts',(2.57029452768271,2.57029390649346,-0.807530151131844));
#7347=CARTESIAN_POINT('Ctrl Pts',(2.59999997971496,2.7786272398268,-0.110862256246237));
#7348=CARTESIAN_POINT('Ctrl Pts',(2.62970543174727,2.98696057316012,0.585805638639234));
#7349=CARTESIAN_POINT('Ctrl Pts',(2.3070971603953,3.19529390649347,1.20399045962738));
#7350=CARTESIAN_POINT('Ctrl Pts',(1.98448888904339,3.40362723982677,1.82217528061537));
#7351=CARTESIAN_POINT('Ctrl Pts',(1.39600952008757,3.61196057316014,2.19623490414904));
#7352=CARTESIAN_POINT('Ctrl Pts',(0.807530151131806,3.82029390649348,2.57029452768262));
#7353=CARTESIAN_POINT('Ctrl Pts',(0.110862256246242,4.0286272398268,2.59999997971498));
#7354=CARTESIAN_POINT('Ctrl Pts',(-0.58580563863932,4.23696057316013,2.62970543174725));
#7355=CARTESIAN_POINT('Ctrl Pts',(-1.2039904596274,4.44529390649346,2.30709716039531));
#7356=CARTESIAN_POINT('Ctrl Pts',(-1.82217528061542,4.6536272398268,1.9844888890433));
#7357=CARTESIAN_POINT('Ctrl Pts',(-2.19623490414908,4.8619605731601,1.39600952008752));
#7358=CARTESIAN_POINT('Ctrl Pts',(-2.57029452768269,5.07029390649345,0.807530151131704));
#7359=CARTESIAN_POINT('Ctrl Pts',(-2.599999979715,5.2786272398268,0.110862256246242));
#7360=CARTESIAN_POINT('Ctrl Pts',(-2.62970543174724,5.48696057316013,-0.585805638639487));
#7361=CARTESIAN_POINT('Ctrl Pts',(-2.30709716039534,5.69529390649347,-1.20399045962746));
#7362=CARTESIAN_POINT('Ctrl Pts',(-1.98448888904338,5.90362723982679,-1.82217528061554));
#7363=CARTESIAN_POINT('Ctrl Pts',(-1.39600952008762,6.11196057316013,-2.19623490414907));
#7364=CARTESIAN_POINT('Ctrl Pts',(-0.807530151131785,6.32029390649347,-2.57029452768279));
#7365=CARTESIAN_POINT('Ctrl Pts',(-0.110862256246242,6.52862723982682,-2.59999997971506));
#7366=CARTESIAN_POINT('Ctrl Pts',(0.585805638639323,6.73696057316013,-2.62970543174735));
#7367=CARTESIAN_POINT('Ctrl Pts',(1.20399045962736,6.94529390649349,-2.3070971603954));
#7368=CARTESIAN_POINT('Ctrl Pts',(1.82217528061547,7.1536272398268,-1.98448888904338));
#7369=CARTESIAN_POINT('Ctrl Pts',(2.19623490414908,7.36196057316014,-1.3960095200876));
#7370=CARTESIAN_POINT('Ctrl Pts',(2.57029452768273,7.5702939064935,-0.807530151131904));
#7371=CARTESIAN_POINT('Ctrl Pts',(2.59999997971498,7.7786272398268,-0.110862256246237));
#7372=CARTESIAN_POINT('Ctrl Pts',(2.62970543174725,7.98696057316015,0.585805638639229));
#7373=CARTESIAN_POINT('Ctrl Pts',(2.3070971603953,8.19529390649346,1.20399045962738));
#7374=CARTESIAN_POINT('Ctrl Pts',(1.9844888890434,8.40362723982681,1.82217528061536));
#7375=CARTESIAN_POINT('Ctrl Pts',(1.39600952008757,8.61196057316016,2.19623490414907));
#7376=CARTESIAN_POINT('Ctrl Pts',(0.807530151131809,8.82029390649348,2.57029452768262));
#7377=CARTESIAN_POINT('Ctrl Pts',(0.110862256246222,9.0286272398268,2.59999997971494));
#7378=CARTESIAN_POINT('Ctrl Pts',(-0.58580563863932,9.23696057316016,2.62970543174721));
#7379=CARTESIAN_POINT('Ctrl Pts',(-1.2039904596274,9.44529390649347,2.30709716039531));
#7380=CARTESIAN_POINT('Ctrl Pts',(-1.82217528061542,9.65362723982683,1.98448888904329));
#7381=CARTESIAN_POINT('Ctrl Pts',(-2.1962349041491,9.86196057316016,1.39600952008751));
#7382=CARTESIAN_POINT('Ctrl Pts',(-2.5702945276827,10.0702939064935,0.80753015113172));
#7383=CARTESIAN_POINT('Ctrl Pts',(-2.59999997971498,10.2786272398268,0.110862256246242));
#7384=CARTESIAN_POINT('Ctrl Pts',(-2.62970543174724,10.4869605731602,-0.585805638639412));
#7385=CARTESIAN_POINT('Ctrl Pts',(-2.30709716039534,10.6952939064935,-1.20399045962747));
#7386=CARTESIAN_POINT('Ctrl Pts',(-1.98448888904336,10.9036272398268,-1.82217528061554));
#7387=CARTESIAN_POINT('Ctrl Pts',(-1.39600952008762,11.1119605731601,-2.19623490414907));
#7388=CARTESIAN_POINT('Ctrl Pts',(-0.807530151131806,11.3202939064935,-2.57029452768279));
#7389=CARTESIAN_POINT('Ctrl Pts',(-0.110862256246242,11.5286272398268,-2.59999997971505));
#7390=CARTESIAN_POINT('Ctrl Pts',(0.585805638639342,11.7369605731602,-2.62970543174735));
#7391=CARTESIAN_POINT('Ctrl Pts',(1.20399045962738,11.9452939064935,-2.3070971603954));
#7392=CARTESIAN_POINT('Ctrl Pts',(1.82217528061545,12.1536272398268,-1.98448888904347));
#7393=CARTESIAN_POINT('Ctrl Pts',(2.19623490414905,12.3619605731601,-1.3960095200876));
#7394=CARTESIAN_POINT('Ctrl Pts',(2.57029452768273,12.5702939064935,-0.807530151131898));
#7395=CARTESIAN_POINT('Ctrl Pts',(2.59999997971498,12.7786272398268,-0.110862256246237));
#7396=CARTESIAN_POINT('Ctrl Pts',(2.62970543174727,12.9869605731601,0.585805638639229));
#7397=CARTESIAN_POINT('Ctrl Pts',(2.3070971603953,13.1952939064935,1.20399045962738));
#7398=CARTESIAN_POINT('Ctrl Pts',(1.98448888904339,13.4036272398268,1.82217528061536));
#7399=CARTESIAN_POINT('Ctrl Pts',(1.39600952008758,13.6119605731601,2.19623490414906));
#7400=CARTESIAN_POINT('Ctrl Pts',(0.807530151131806,13.8202939064935,2.57029452768263));
#7401=CARTESIAN_POINT('Ctrl Pts',(0.110862256246242,14.0286272398268,2.59999997971497));
#7402=CARTESIAN_POINT('Ctrl Pts',(-0.585805638639299,14.2369605731602,2.62970543174722));
#7403=CARTESIAN_POINT('Ctrl Pts',(-1.20399045962738,14.4452939064935,2.30709716039531));
#7404=CARTESIAN_POINT('Ctrl Pts',(-1.82217528061545,14.6536272398268,1.9844888890433));
#7405=CARTESIAN_POINT('Ctrl Pts',(-2.19623490414908,14.8619605731602,1.39600952008751));
#7406=CARTESIAN_POINT('Ctrl Pts',(-2.57029452768271,15.0702939064935,0.807530151131736));
#7407=CARTESIAN_POINT('Ctrl Pts',(-2.59999997971498,15.2786272398268,0.110862256246242));
#7408=CARTESIAN_POINT('Ctrl Pts',(-2.62970543174723,15.4869605731602,-0.585805638639412));
#7409=CARTESIAN_POINT('Ctrl Pts',(-2.30709716039532,15.6952939064935,-1.20399045962746));
#7410=CARTESIAN_POINT('Ctrl Pts',(-1.98448888904338,15.9036272398268,-1.82217528061553));
#7411=CARTESIAN_POINT('Ctrl Pts',(-1.39600952008762,16.1119605731601,-2.19623490414907));
#7412=CARTESIAN_POINT('Ctrl Pts',(-0.807530151131785,16.3202939064935,-2.57029452768285));
#7413=CARTESIAN_POINT('Ctrl Pts',(-0.110862256246242,16.5286272398268,-2.59999997971506));
#7414=CARTESIAN_POINT('Ctrl Pts',(0.585805638639345,16.7369605731602,-2.62970543174732));
#7415=CARTESIAN_POINT('Ctrl Pts',(1.20399045962736,16.9452939064935,-2.3070971603954));
#7416=CARTESIAN_POINT('Ctrl Pts',(1.82217528061547,17.1536272398268,-1.98448888904346));
#7417=CARTESIAN_POINT('Ctrl Pts',(2.19623490414905,17.3619605731602,-1.3960095200876));
#7418=CARTESIAN_POINT('Ctrl Pts',(2.57029452768272,17.5702939064935,-0.807530151131855));
#7419=CARTESIAN_POINT('Ctrl Pts',(2.59999997971496,17.7786272398268,-0.110862256246237));
#7420=CARTESIAN_POINT('Ctrl Pts',(2.62970543174727,17.9869605731602,0.58580563863925));
#7421=CARTESIAN_POINT('Ctrl Pts',(2.3070971603953,18.1952939064935,1.20399045962738));
#7422=CARTESIAN_POINT('Ctrl Pts',(1.98448888904339,18.4036272398268,1.82217528061535));
#7423=CARTESIAN_POINT('Ctrl Pts',(1.39600952008758,18.6119605731602,2.19623490414907));
#7424=CARTESIAN_POINT('Ctrl Pts',(0.807530151131809,18.8202939064935,2.57029452768262));
#7425=CARTESIAN_POINT('Ctrl Pts',(0.110862256246222,19.0286272398268,2.59999997971497));
#7426=CARTESIAN_POINT('Ctrl Pts',(-0.58580563863932,19.2369605731602,2.62970543174719));
#7427=CARTESIAN_POINT('Ctrl Pts',(-1.2039904596274,19.4452939064935,2.30709716039531));
#7428=CARTESIAN_POINT('Ctrl Pts',(-1.82217528061545,19.6536272398268,1.98448888904328));
#7429=CARTESIAN_POINT('Ctrl Pts',(-2.1962349041491,19.8619605731602,1.39600952008757));
#7430=CARTESIAN_POINT('Ctrl Pts',(-2.57029452768269,20.0702939064935,0.807530151131736));
#7431=CARTESIAN_POINT('Ctrl Pts',(-2.59999997971498,20.2786272398269,0.110862256246232));
#7432=CARTESIAN_POINT('Ctrl Pts',(-2.62970543174724,20.4869605731602,-0.58580563863938));
#7433=CARTESIAN_POINT('Ctrl Pts',(-2.30709716039534,20.6952939064935,-1.20399045962747));
#7434=CARTESIAN_POINT('Ctrl Pts',(-1.98448888904338,20.9036272398268,-1.82217528061549));
#7435=CARTESIAN_POINT('Ctrl Pts',(-1.3960095200876,21.1119605731601,-2.19623490414907));
#7436=CARTESIAN_POINT('Ctrl Pts',(-0.807530151131806,21.3202939064935,-2.5702945276828));
#7437=CARTESIAN_POINT('Ctrl Pts',(-0.110862256246263,21.5286272398268,-2.59999997971503));
#7438=CARTESIAN_POINT('Ctrl Pts',(0.585805638639342,21.7369605731602,-2.62970543174737));
#7439=CARTESIAN_POINT('Ctrl Pts',(1.20399045962736,21.9452939064935,-2.3070971603954));
#7440=CARTESIAN_POINT('Ctrl Pts',(1.82217528061545,22.1536272398268,-1.98448888904342));
#7441=CARTESIAN_POINT('Ctrl Pts',(2.19623490414905,22.3619605731602,-1.39600952008764));
#7442=CARTESIAN_POINT('Ctrl Pts',(2.57029452768271,22.5702939064935,-0.807530151131882));
#7443=CARTESIAN_POINT('Ctrl Pts',(2.59999997971498,22.7786272398268,-0.110862256246242));
#7444=CARTESIAN_POINT('Ctrl Pts',(2.62970543174725,22.9869605731602,0.585805638639224));
#7445=CARTESIAN_POINT('Ctrl Pts',(2.30709716039531,23.1952939064935,1.20399045962736));
#7446=CARTESIAN_POINT('Ctrl Pts',(1.98448888904341,23.4036272398269,1.82217528061539));
#7447=CARTESIAN_POINT('Ctrl Pts',(1.39600952008758,23.6119605731602,2.19623490414907));
#7448=CARTESIAN_POINT('Ctrl Pts',(0.807530151131828,23.8202939064935,2.57029452768264));
#7449=CARTESIAN_POINT('Ctrl Pts',(0.110862256246222,24.0286272398268,2.59999997971497));
#7450=CARTESIAN_POINT('Ctrl Pts',(-0.585805638639299,24.2369605731602,2.62970543174718));
#7451=CARTESIAN_POINT('Ctrl Pts',(-1.2039904596274,24.4452939064935,2.30709716039532));
#7452=CARTESIAN_POINT('Ctrl Pts',(-1.82217528061544,24.6536272398269,1.9844888890433));
#7453=CARTESIAN_POINT('Ctrl Pts',(-2.19623490414908,24.8619605731602,1.39600952008758));
#7454=CARTESIAN_POINT('Ctrl Pts',(-2.5702945276827,25.0702939064935,0.807530151131763));
#7455=CARTESIAN_POINT('Ctrl Pts',(-2.59999997971498,25.2786272398269,0.110862256246232));
#7456=CARTESIAN_POINT('Ctrl Pts',(-2.62970543174725,25.4869605731602,-0.58580563863938));
#7457=CARTESIAN_POINT('Ctrl Pts',(-2.30709716039532,25.6952939064935,-1.20399045962744));
#7458=CARTESIAN_POINT('Ctrl Pts',(-1.98448888904338,25.9036272398269,-1.82217528061553));
#7459=CARTESIAN_POINT('Ctrl Pts',(-1.39600952008761,26.1119605731602,-2.19623490414911));
#7460=CARTESIAN_POINT('Ctrl Pts',(-0.807530151131806,26.3202939064935,-2.57029452768279));
#7461=CARTESIAN_POINT('Ctrl Pts',(-0.110862256246242,26.5286272398269,-2.59999997971503));
#7462=CARTESIAN_POINT('Ctrl Pts',(0.585805638639323,26.7369605731602,-2.62970543174736));
#7463=CARTESIAN_POINT('Ctrl Pts',(1.20399045962738,26.9452939064935,-2.30709716039544));
#7464=CARTESIAN_POINT('Ctrl Pts',(1.82217528061545,27.1536272398269,-1.98448888904342));
#7465=CARTESIAN_POINT('Ctrl Pts',(2.19623490414907,27.3619605731602,-1.39600952008769));
#7466=CARTESIAN_POINT('Ctrl Pts',(2.5702945276827,27.5702939064935,-0.807530151131893));
#7467=CARTESIAN_POINT('Ctrl Pts',(2.59999997971496,27.7786272398269,-0.110862256246331));
#7468=CARTESIAN_POINT('Ctrl Pts',(2.62970543174725,27.9869605731602,0.58580563863925));
#7469=CARTESIAN_POINT('Ctrl Pts',(2.30709716039531,28.1952939064935,1.20399045962735));
#7470=CARTESIAN_POINT('Ctrl Pts',(1.98448888904339,28.4036272398269,1.82217528061536));
#7471=CARTESIAN_POINT('Ctrl Pts',(1.39600952008758,28.6119605731601,2.19623490414907));
#7472=CARTESIAN_POINT('Ctrl Pts',(0.807530151131809,28.8202939064936,2.57029452768262));
#7473=CARTESIAN_POINT('Ctrl Pts',(0.110862256246242,29.0286272398268,2.59999997971497));
#7474=CARTESIAN_POINT('Ctrl Pts',(-0.58580563863932,29.2369605731602,2.6297054317472));
#7475=CARTESIAN_POINT('Ctrl Pts',(-1.2039904596274,29.4452939064935,2.30709716039532));
#7476=CARTESIAN_POINT('Ctrl Pts',(-1.82217528061545,29.6536272398269,1.98448888904329));
#7477=CARTESIAN_POINT('Ctrl Pts',(-2.19623490414908,29.8619605731602,1.39600952008757));
#7478=CARTESIAN_POINT('Ctrl Pts',(-2.5702945276827,30.0702939064936,0.807530151131736));
#7479=CARTESIAN_POINT('Ctrl Pts',(-2.59999997971498,30.2786272398269,0.110862256246195));
#7480=CARTESIAN_POINT('Ctrl Pts',(-2.62970543174725,30.4869605731602,-0.585805638639385));
#7481=CARTESIAN_POINT('Ctrl Pts',(-2.30709716039534,30.6952939064935,-1.20399045962744));
#7482=CARTESIAN_POINT('Ctrl Pts',(-1.98448888904338,30.9036272398269,-1.82217528061551));
#7483=CARTESIAN_POINT('Ctrl Pts',(-1.3960095200876,31.1119605731602,-2.19623490414911));
#7484=CARTESIAN_POINT('Ctrl Pts',(-0.807530151131806,31.3202939064935,-2.57029452768284));
#7485=CARTESIAN_POINT('Ctrl Pts',(-0.110862256246242,31.5286272398269,-2.59999997971504));
#7486=CARTESIAN_POINT('Ctrl Pts',(0.585805638639323,31.7369605731602,-2.62970543174734));
#7487=CARTESIAN_POINT('Ctrl Pts',(1.20399045962736,31.9452939064936,-2.30709716039543));
#7488=CARTESIAN_POINT('Ctrl Pts',(1.82217528061545,32.1536272398269,-1.98448888904345));
#7489=CARTESIAN_POINT('Ctrl Pts',(2.19623490414904,32.3619605731602,-1.39600952008769));
#7490=CARTESIAN_POINT('Ctrl Pts',(2.57029452768271,32.5702939064935,-0.807530151131882));
#7491=CARTESIAN_POINT('Ctrl Pts',(2.59999997971498,32.7786272398269,-0.110862256246289));
#7492=CARTESIAN_POINT('Ctrl Pts',(2.62970543174725,32.9869605731603,0.585805638639218));
#7493=CARTESIAN_POINT('Ctrl Pts',(2.30709716039531,33.1952939064935,1.20399045962734));
#7494=CARTESIAN_POINT('Ctrl Pts',(1.98448888904338,33.4036272398269,1.82217528061539));
#7495=CARTESIAN_POINT('Ctrl Pts',(1.3960095200876,33.6119605731602,2.19623490414906));
#7496=CARTESIAN_POINT('Ctrl Pts',(0.807530151131828,33.8202939064936,2.57029452768264));
#7497=CARTESIAN_POINT('Ctrl Pts',(0.110862256246222,34.0286272398269,2.59999997971497));
#7498=CARTESIAN_POINT('Ctrl Pts',(-0.585805638639323,34.2369605731602,2.62970543174719));
#7499=CARTESIAN_POINT('Ctrl Pts',(-1.2039904596274,34.4452939064935,2.30709716039531));
#7500=CARTESIAN_POINT('Ctrl Pts',(-1.82217528061545,34.6536272398269,1.9844888890433));
#7501=CARTESIAN_POINT('Ctrl Pts',(-2.1962349041491,34.8619605731602,1.39600952008757));
#7502=CARTESIAN_POINT('Ctrl Pts',(-2.5702945276827,35.0702939064936,0.807530151131747));
#7503=CARTESIAN_POINT('Ctrl Pts',(-2.59999997971498,35.2786272398269,0.110862256246206));
#7504=CARTESIAN_POINT('Ctrl Pts',(-2.62970543174723,35.4869605731602,-0.585805638639401));
#7505=CARTESIAN_POINT('Ctrl Pts',(-2.30709716039534,35.6952939064935,-1.20399045962745));
#7506=CARTESIAN_POINT('Ctrl Pts',(-1.98448888904336,35.9036272398269,-1.82217528061553));
#7507=CARTESIAN_POINT('Ctrl Pts',(-1.3960095200876,36.1119605731602,-2.19623490414911));
#7508=CARTESIAN_POINT('Ctrl Pts',(-0.807530151131785,36.3202939064935,-2.5702945276828));
#7509=CARTESIAN_POINT('Ctrl Pts',(-0.110862256246263,36.5286272398269,-2.59999997971503));
#7510=CARTESIAN_POINT('Ctrl Pts',(0.585805638639323,36.7369605731602,-2.62970543174736));
#7511=CARTESIAN_POINT('Ctrl Pts',(1.20399045962738,36.9452939064935,-2.30709716039542));
#7512=CARTESIAN_POINT('Ctrl Pts',(1.82217528061547,37.1536272398269,-1.98448888904344));
#7513=CARTESIAN_POINT('Ctrl Pts',(2.19623490414907,37.3619605731602,-1.39600952008768));
#7514=CARTESIAN_POINT('Ctrl Pts',(2.57029452768271,37.5702939064935,-0.807530151131898));
#7515=CARTESIAN_POINT('Ctrl Pts',(2.59999997971498,37.7786272398269,-0.110862256246305));
#7516=CARTESIAN_POINT('Ctrl Pts',(2.62970543174725,37.9869605731602,0.585805638639256));
#7517=CARTESIAN_POINT('Ctrl Pts',(2.30709716039532,38.1952939064936,1.20399045962733));
#7518=CARTESIAN_POINT('Ctrl Pts',(1.98448888904339,38.4036272398269,1.82217528061537));
#7519=CARTESIAN_POINT('Ctrl Pts',(1.3960095200876,38.6119605731602,2.19623490414906));
#7520=CARTESIAN_POINT('Ctrl Pts',(0.807530151131828,38.8202939064936,2.57029452768263));
#7521=CARTESIAN_POINT('Ctrl Pts',(0.110862256246222,39.0286272398269,2.59999997971497));
#7522=CARTESIAN_POINT('Ctrl Pts',(-0.58580563863932,39.2369605731602,2.62970543174721));
#7523=CARTESIAN_POINT('Ctrl Pts',(-1.2039904596274,39.4452939064936,2.30709716039531));
#7524=CARTESIAN_POINT('Ctrl Pts',(-1.82217528061542,39.6536272398269,1.98448888904328));
#7525=CARTESIAN_POINT('Ctrl Pts',(-2.19623490414908,39.8619605731602,1.39600952008758));
#7526=CARTESIAN_POINT('Ctrl Pts',(-2.5702945276827,40.0702939064936,0.807530151131726));
#7527=CARTESIAN_POINT('Ctrl Pts',(-2.59999997971498,40.2786272398269,0.110862256246201));
#7528=CARTESIAN_POINT('Ctrl Pts',(-2.00006370137914,0.278745603789511,0.110909351770506));
#7529=CARTESIAN_POINT('Ctrl Pts',(-2.02978177261913,0.487078937122742,-0.425006101824765));
#7530=CARTESIAN_POINT('Ctrl Pts',(-1.78756065046676,0.695412270456132,-0.903981534539017));
#7531=CARTESIAN_POINT('Ctrl Pts',(-1.5453395283144,0.903745603789377,-1.38295696725319));
#7532=CARTESIAN_POINT('Ctrl Pts',(-1.09608216684017,1.11207893712281,-1.67665129869622));
#7533=CARTESIAN_POINT('Ctrl Pts',(-0.646824805365941,1.32041227045615,-1.97034563013915));
#7534=CARTESIAN_POINT('Ctrl Pts',(-0.110909351770586,1.52874560378948,-2.00006370137914));
#7535=CARTESIAN_POINT('Ctrl Pts',(0.425006101824744,1.73707893712275,-2.02978177261916));
#7536=CARTESIAN_POINT('Ctrl Pts',(0.903981534538964,1.94541227045615,-1.78756065046677));
#7537=CARTESIAN_POINT('Ctrl Pts',(1.38295696725319,2.15374560378948,-1.5453395283144));
#7538=CARTESIAN_POINT('Ctrl Pts',(1.67665129869617,2.36207893712281,-1.09608216684018));
#7539=CARTESIAN_POINT('Ctrl Pts',(1.97034563013914,2.57041227045613,-0.646824805365955));
#7540=CARTESIAN_POINT('Ctrl Pts',(2.00006370137916,2.77874560378949,-0.110909351770603));
#7541=CARTESIAN_POINT('Ctrl Pts',(2.02978177261913,2.98707893712281,0.425006101824722));
#7542=CARTESIAN_POINT('Ctrl Pts',(1.78756065046677,3.19541227045615,0.903981534538913));
#7543=CARTESIAN_POINT('Ctrl Pts',(1.5453395283144,3.40374560378943,1.38295696725317));
#7544=CARTESIAN_POINT('Ctrl Pts',(1.09608216684017,3.61207893712282,1.67665129869616));
#7545=CARTESIAN_POINT('Ctrl Pts',(0.646824805365943,3.8204122704561,1.97034563013913));
#7546=CARTESIAN_POINT('Ctrl Pts',(0.1109093517706,4.02874560378949,2.00006370137908));
#7547=CARTESIAN_POINT('Ctrl Pts',(-0.425006101824727,4.23707893712277,2.02978177261911));
#7548=CARTESIAN_POINT('Ctrl Pts',(-0.903981534538964,4.44541227045615,1.78756065046676));
#7549=CARTESIAN_POINT('Ctrl Pts',(-1.38295696725319,4.65374560378948,1.54533952831435));
#7550=CARTESIAN_POINT('Ctrl Pts',(-1.67665129869618,4.86207893712285,1.09608216684011));
#7551=CARTESIAN_POINT('Ctrl Pts',(-1.97034563013914,5.07041227045609,0.646824805365927));
#7552=CARTESIAN_POINT('Ctrl Pts',(-2.00006370137914,5.27874560378947,0.110909351770506));
#7553=CARTESIAN_POINT('Ctrl Pts',(-2.02978177261913,5.48707893712276,-0.425006101824808));
#7554=CARTESIAN_POINT('Ctrl Pts',(-1.78756065046676,5.69541227045614,-0.903981534539017));
#7555=CARTESIAN_POINT('Ctrl Pts',(-1.5453395283144,5.90374560378943,-1.38295696725317));
#7556=CARTESIAN_POINT('Ctrl Pts',(-1.09608216684016,6.11207893712282,-1.67665129869616));
#7557=CARTESIAN_POINT('Ctrl Pts',(-0.646824805365928,6.32041227045614,-1.97034563013915));
#7558=CARTESIAN_POINT('Ctrl Pts',(-0.110909351770598,6.52874560378952,-2.00006370137919));
#7559=CARTESIAN_POINT('Ctrl Pts',(0.425006101824742,6.73707893712276,-2.02978177261914));
#7560=CARTESIAN_POINT('Ctrl Pts',(0.903981534538965,6.94541227045619,-1.78756065046677));
#7561=CARTESIAN_POINT('Ctrl Pts',(1.3829569672532,7.15374560378946,-1.54533952831446));
#7562=CARTESIAN_POINT('Ctrl Pts',(1.67665129869614,7.36207893712281,-1.09608216684023));
#7563=CARTESIAN_POINT('Ctrl Pts',(1.97034563013915,7.57041227045615,-0.646824805365941));
#7564=CARTESIAN_POINT('Ctrl Pts',(2.00006370137914,7.77874560378953,-0.11090935177061));
#7565=CARTESIAN_POINT('Ctrl Pts',(2.02978177261913,7.98707893712276,0.425006101824722));
#7566=CARTESIAN_POINT('Ctrl Pts',(1.78756065046677,8.19541227045616,0.903981534538955));
#7567=CARTESIAN_POINT('Ctrl Pts',(1.54533952831442,8.40374560378946,1.38295696725319));
#7568=CARTESIAN_POINT('Ctrl Pts',(1.09608216684017,8.61207893712284,1.67665129869611));
#7569=CARTESIAN_POINT('Ctrl Pts',(0.646824805365943,8.82041227045615,1.97034563013914));
#7570=CARTESIAN_POINT('Ctrl Pts',(0.110909351770597,9.0287456037895,2.00006370137908));
#7571=CARTESIAN_POINT('Ctrl Pts',(-0.42500610182474,9.23707893712282,2.02978177261913));
#7572=CARTESIAN_POINT('Ctrl Pts',(-0.903981534538962,9.44541227045615,1.78756065046671));
#7573=CARTESIAN_POINT('Ctrl Pts',(-1.38295696725319,9.65374560378948,1.5453395283144));
#7574=CARTESIAN_POINT('Ctrl Pts',(-1.67665129869616,9.86207893712282,1.09608216684017));
#7575=CARTESIAN_POINT('Ctrl Pts',(-1.97034563013914,10.0704122704562,0.646824805365941));
#7576=CARTESIAN_POINT('Ctrl Pts',(-2.00006370137912,10.2787456037895,0.110909351770534));
#7577=CARTESIAN_POINT('Ctrl Pts',(-2.02978177261913,10.4870789371228,-0.425006101824744));
#7578=CARTESIAN_POINT('Ctrl Pts',(-1.78756065046676,10.6954122704562,-0.903981534539066));
#7579=CARTESIAN_POINT('Ctrl Pts',(-1.5453395283144,10.9037456037894,-1.3829569672532));
#7580=CARTESIAN_POINT('Ctrl Pts',(-1.09608216684017,11.1120789371228,-1.67665129869622));
#7581=CARTESIAN_POINT('Ctrl Pts',(-0.646824805365941,11.3204122704561,-1.97034563013915));
#7582=CARTESIAN_POINT('Ctrl Pts',(-0.1109093517706,11.5287456037895,-2.00006370137916));
#7583=CARTESIAN_POINT('Ctrl Pts',(0.425006101824742,11.7370789371228,-2.02978177261915));
#7584=CARTESIAN_POINT('Ctrl Pts',(0.903981534538964,11.9454122704562,-1.78756065046677));
#7585=CARTESIAN_POINT('Ctrl Pts',(1.38295696725319,12.1537456037895,-1.54533952831446));
#7586=CARTESIAN_POINT('Ctrl Pts',(1.67665129869616,12.3620789371228,-1.09608216684018));
#7587=CARTESIAN_POINT('Ctrl Pts',(1.97034563013917,12.5704122704561,-0.646824805365955));
#7588=CARTESIAN_POINT('Ctrl Pts',(2.00006370137914,12.7787456037895,-0.110909351770652));
#7589=CARTESIAN_POINT('Ctrl Pts',(2.02978177261913,12.9870789371228,0.425006101824744));
#7590=CARTESIAN_POINT('Ctrl Pts',(1.78756065046676,13.1954122704562,0.903981534538906));
#7591=CARTESIAN_POINT('Ctrl Pts',(1.5453395283144,13.4037456037895,1.38295696725318));
#7592=CARTESIAN_POINT('Ctrl Pts',(1.09608216684017,13.6120789371228,1.67665129869616));
#7593=CARTESIAN_POINT('Ctrl Pts',(0.646824805365943,13.8204122704562,1.97034563013915));
#7594=CARTESIAN_POINT('Ctrl Pts',(0.1109093517706,14.0287456037895,2.0000637013791));
#7595=CARTESIAN_POINT('Ctrl Pts',(-0.425006101824742,14.2370789371228,2.02978177261913));
#7596=CARTESIAN_POINT('Ctrl Pts',(-0.903981534538964,14.4454122704562,1.78756065046667));
#7597=CARTESIAN_POINT('Ctrl Pts',(-1.38295696725319,14.6537456037895,1.54533952831435));
#7598=CARTESIAN_POINT('Ctrl Pts',(-1.67665129869616,14.8620789371229,1.09608216684011));
#7599=CARTESIAN_POINT('Ctrl Pts',(-1.97034563013913,15.0704122704562,0.646824805365955));
#7600=CARTESIAN_POINT('Ctrl Pts',(-2.00006370137914,15.2787456037895,0.110909351770541));
#7601=CARTESIAN_POINT('Ctrl Pts',(-2.02978177261913,15.4870789371228,-0.425006101824851));
#7602=CARTESIAN_POINT('Ctrl Pts',(-1.78756065046676,15.6954122704562,-0.903981534538976));
#7603=CARTESIAN_POINT('Ctrl Pts',(-1.5453395283144,15.9037456037895,-1.38295696725319));
#7604=CARTESIAN_POINT('Ctrl Pts',(-1.09608216684016,16.1120789371229,-1.6766512986962));
#7605=CARTESIAN_POINT('Ctrl Pts',(-0.646824805365941,16.3204122704561,-1.9703456301392));
#7606=CARTESIAN_POINT('Ctrl Pts',(-0.1109093517706,16.5287456037895,-2.00006370137919));
#7607=CARTESIAN_POINT('Ctrl Pts',(0.425006101824744,16.7370789371228,-2.02978177261913));
#7608=CARTESIAN_POINT('Ctrl Pts',(0.903981534538977,16.9454122704562,-1.78756065046677));
#7609=CARTESIAN_POINT('Ctrl Pts',(1.38295696725319,17.1537456037895,-1.5453395283144));
#7610=CARTESIAN_POINT('Ctrl Pts',(1.67665129869616,17.3620789371229,-1.09608216684022));
#7611=CARTESIAN_POINT('Ctrl Pts',(1.97034563013914,17.5704122704561,-0.646824805365941));
#7612=CARTESIAN_POINT('Ctrl Pts',(2.00006370137914,17.7787456037895,-0.11090935177061));
#7613=CARTESIAN_POINT('Ctrl Pts',(2.02978177261913,17.9870789371228,0.425006101824686));
#7614=CARTESIAN_POINT('Ctrl Pts',(1.78756065046677,18.1954122704562,0.903981534538948));
#7615=CARTESIAN_POINT('Ctrl Pts',(1.54533952831442,18.4037456037895,1.38295696725319));
#7616=CARTESIAN_POINT('Ctrl Pts',(1.09608216684017,18.6120789371228,1.67665129869611));
#7617=CARTESIAN_POINT('Ctrl Pts',(0.646824805365943,18.8204122704562,1.97034563013914));
#7618=CARTESIAN_POINT('Ctrl Pts',(0.110909351770598,19.0287456037895,2.00006370137909));
#7619=CARTESIAN_POINT('Ctrl Pts',(-0.425006101824742,19.2370789371228,2.02978177261913));
#7620=CARTESIAN_POINT('Ctrl Pts',(-0.903981534538962,19.4454122704562,1.78756065046669));
#7621=CARTESIAN_POINT('Ctrl Pts',(-1.38295696725319,19.6537456037895,1.5453395283144));
#7622=CARTESIAN_POINT('Ctrl Pts',(-1.67665129869616,19.8620789371228,1.09608216684013));
#7623=CARTESIAN_POINT('Ctrl Pts',(-1.97034563013915,20.0704122704561,0.646824805365941));
#7624=CARTESIAN_POINT('Ctrl Pts',(-2.00006370137912,20.2787456037895,0.110909351770513));
#7625=CARTESIAN_POINT('Ctrl Pts',(-2.02978177261911,20.4870789371228,-0.425006101824801));
#7626=CARTESIAN_POINT('Ctrl Pts',(-1.78756065046676,20.6954122704562,-0.903981534539024));
#7627=CARTESIAN_POINT('Ctrl Pts',(-1.54533952831439,20.9037456037895,-1.38295696725322));
#7628=CARTESIAN_POINT('Ctrl Pts',(-1.09608216684018,21.1120789371229,-1.67665129869622));
#7629=CARTESIAN_POINT('Ctrl Pts',(-0.646824805365943,21.3204122704561,-1.97034563013915));
#7630=CARTESIAN_POINT('Ctrl Pts',(-0.1109093517706,21.5287456037895,-2.00006370137914));
#7631=CARTESIAN_POINT('Ctrl Pts',(0.425006101824742,21.7370789371228,-2.02978177261912));
#7632=CARTESIAN_POINT('Ctrl Pts',(0.903981534538964,21.9454122704562,-1.7875606504668));
#7633=CARTESIAN_POINT('Ctrl Pts',(1.38295696725319,22.1537456037895,-1.54533952831446));
#7634=CARTESIAN_POINT('Ctrl Pts',(1.67665129869617,22.3620789371229,-1.09608216684019));
#7635=CARTESIAN_POINT('Ctrl Pts',(1.97034563013912,22.5704122704561,-0.646824805365941));
#7636=CARTESIAN_POINT('Ctrl Pts',(2.00006370137914,22.7787456037895,-0.110909351770638));
#7637=CARTESIAN_POINT('Ctrl Pts',(2.02978177261915,22.9870789371228,0.425006101824744));
#7638=CARTESIAN_POINT('Ctrl Pts',(1.78756065046677,23.1954122704562,0.903981534538906));
#7639=CARTESIAN_POINT('Ctrl Pts',(1.5453395283144,23.4037456037895,1.38295696725318));
#7640=CARTESIAN_POINT('Ctrl Pts',(1.09608216684017,23.6120789371229,1.67665129869614));
#7641=CARTESIAN_POINT('Ctrl Pts',(0.646824805365957,23.8204122704561,1.97034563013915));
#7642=CARTESIAN_POINT('Ctrl Pts',(0.1109093517706,24.0287456037895,2.00006370137905));
#7643=CARTESIAN_POINT('Ctrl Pts',(-0.425006101824742,24.2370789371228,2.02978177261914));
#7644=CARTESIAN_POINT('Ctrl Pts',(-0.903981534538964,24.4454122704562,1.78756065046667));
#7645=CARTESIAN_POINT('Ctrl Pts',(-1.38295696725317,24.6537456037895,1.54533952831433));
#7646=CARTESIAN_POINT('Ctrl Pts',(-1.67665129869615,24.8620789371229,1.09608216684012));
#7647=CARTESIAN_POINT('Ctrl Pts',(-1.97034563013914,25.0704122704562,0.646824805365955));
#7648=CARTESIAN_POINT('Ctrl Pts',(-2.00006370137914,25.2787456037895,0.110909351770548));
#7649=CARTESIAN_POINT('Ctrl Pts',(-2.02978177261913,25.4870789371228,-0.425006101824772));
#7650=CARTESIAN_POINT('Ctrl Pts',(-1.78756065046676,25.6954122704562,-0.903981534538976));
#7651=CARTESIAN_POINT('Ctrl Pts',(-1.5453395283144,25.9037456037895,-1.38295696725319));
#7652=CARTESIAN_POINT('Ctrl Pts',(-1.09608216684017,26.1120789371229,-1.67665129869619));
#7653=CARTESIAN_POINT('Ctrl Pts',(-0.646824805365941,26.3204122704561,-1.9703456301392));
#7654=CARTESIAN_POINT('Ctrl Pts',(-0.1109093517706,26.5287456037895,-2.00006370137917));
#7655=CARTESIAN_POINT('Ctrl Pts',(0.425006101824756,26.7370789371228,-2.02978177261913));
#7656=CARTESIAN_POINT('Ctrl Pts',(0.903981534538977,26.9454122704562,-1.78756065046682));
#7657=CARTESIAN_POINT('Ctrl Pts',(1.38295696725319,27.1537456037895,-1.5453395283144));
#7658=CARTESIAN_POINT('Ctrl Pts',(1.67665129869614,27.3620789371229,-1.09608216684021));
#7659=CARTESIAN_POINT('Ctrl Pts',(1.97034563013914,27.5704122704562,-0.646824805365969));
#7660=CARTESIAN_POINT('Ctrl Pts',(2.00006370137911,27.7787456037896,-0.110909351770603));
#7661=CARTESIAN_POINT('Ctrl Pts',(2.02978177261913,27.9870789371228,0.425006101824736));
#7662=CARTESIAN_POINT('Ctrl Pts',(1.78756065046677,28.1954122704562,0.903981534538934));
#7663=CARTESIAN_POINT('Ctrl Pts',(1.54533952831439,28.4037456037895,1.38295696725318));
#7664=CARTESIAN_POINT('Ctrl Pts',(1.09608216684017,28.6120789371229,1.67665129869612));
#7665=CARTESIAN_POINT('Ctrl Pts',(0.646824805365943,28.8204122704562,1.97034563013911));
#7666=CARTESIAN_POINT('Ctrl Pts',(0.110909351770614,29.0287456037896,2.0000637013791));
#7667=CARTESIAN_POINT('Ctrl Pts',(-0.425006101824742,29.2370789371228,2.02978177261913));
#7668=CARTESIAN_POINT('Ctrl Pts',(-0.903981534538962,29.4454122704562,1.78756065046671));
#7669=CARTESIAN_POINT('Ctrl Pts',(-1.38295696725319,29.6537456037896,1.54533952831437));
#7670=CARTESIAN_POINT('Ctrl Pts',(-1.67665129869616,29.8620789371229,1.0960821668401));
#7671=CARTESIAN_POINT('Ctrl Pts',(-1.97034563013914,30.0704122704562,0.646824805365912));
#7672=CARTESIAN_POINT('Ctrl Pts',(-2.00006370137914,30.2787456037896,0.110909351770527));
#7673=CARTESIAN_POINT('Ctrl Pts',(-2.02978177261913,30.4870789371228,-0.425006101824801));
#7674=CARTESIAN_POINT('Ctrl Pts',(-1.78756065046675,30.6954122704562,-0.90398153453901));
#7675=CARTESIAN_POINT('Ctrl Pts',(-1.5453395283144,30.9037456037895,-1.38295696725315));
#7676=CARTESIAN_POINT('Ctrl Pts',(-1.09608216684017,31.1120789371229,-1.67665129869622));
#7677=CARTESIAN_POINT('Ctrl Pts',(-0.646824805365941,31.3204122704562,-1.97034563013915));
#7678=CARTESIAN_POINT('Ctrl Pts',(-0.110909351770598,31.5287456037896,-2.00006370137914));
#7679=CARTESIAN_POINT('Ctrl Pts',(0.425006101824744,31.7370789371229,-2.02978177261914));
#7680=CARTESIAN_POINT('Ctrl Pts',(0.903981534538951,31.9454122704562,-1.78756065046679));
#7681=CARTESIAN_POINT('Ctrl Pts',(1.38295696725319,32.1537456037895,-1.54533952831446));
#7682=CARTESIAN_POINT('Ctrl Pts',(1.67665129869616,32.3620789371229,-1.09608216684022));
#7683=CARTESIAN_POINT('Ctrl Pts',(1.97034563013914,32.5704122704561,-0.646824805365941));
#7684=CARTESIAN_POINT('Ctrl Pts',(2.00006370137914,32.7787456037896,-0.11090935177061));
#7685=CARTESIAN_POINT('Ctrl Pts',(2.02978177261913,32.9870789371229,0.425006101824715));
#7686=CARTESIAN_POINT('Ctrl Pts',(1.78756065046676,33.1954122704563,0.903981534538906));
#7687=CARTESIAN_POINT('Ctrl Pts',(1.5453395283144,33.4037456037895,1.3829569672532));
#7688=CARTESIAN_POINT('Ctrl Pts',(1.09608216684017,33.6120789371229,1.67665129869615));
#7689=CARTESIAN_POINT('Ctrl Pts',(0.646824805365943,33.8204122704562,1.97034563013915));
#7690=CARTESIAN_POINT('Ctrl Pts',(0.1109093517706,34.0287456037896,2.00006370137906));
#7691=CARTESIAN_POINT('Ctrl Pts',(-0.425006101824742,34.2370789371229,2.02978177261912));
#7692=CARTESIAN_POINT('Ctrl Pts',(-0.903981534538964,34.4454122704562,1.7875606504667));
#7693=CARTESIAN_POINT('Ctrl Pts',(-1.3829569672532,34.6537456037895,1.54533952831438));
#7694=CARTESIAN_POINT('Ctrl Pts',(-1.67665129869615,34.8620789371228,1.09608216684013));
#7695=CARTESIAN_POINT('Ctrl Pts',(-1.97034563013914,35.0704122704562,0.646824805365955));
#7696=CARTESIAN_POINT('Ctrl Pts',(-2.00006370137914,35.2787456037896,0.110909351770548));
#7697=CARTESIAN_POINT('Ctrl Pts',(-2.02978177261913,35.4870789371229,-0.425006101824787));
#7698=CARTESIAN_POINT('Ctrl Pts',(-1.78756065046676,35.6954122704562,-0.903981534538996));
#7699=CARTESIAN_POINT('Ctrl Pts',(-1.5453395283144,35.9037456037895,-1.3829569672532));
#7700=CARTESIAN_POINT('Ctrl Pts',(-1.09608216684017,36.1120789371229,-1.67665129869619));
#7701=CARTESIAN_POINT('Ctrl Pts',(-0.646824805365928,36.3204122704562,-1.97034563013915));
#7702=CARTESIAN_POINT('Ctrl Pts',(-0.1109093517706,36.5287456037896,-2.00006370137918));
#7703=CARTESIAN_POINT('Ctrl Pts',(0.425006101824742,36.7370789371229,-2.02978177261914));
#7704=CARTESIAN_POINT('Ctrl Pts',(0.903981534538964,36.9454122704562,-1.78756065046682));
#7705=CARTESIAN_POINT('Ctrl Pts',(1.38295696725319,37.1537456037895,-1.5453395283144));
#7706=CARTESIAN_POINT('Ctrl Pts',(1.67665129869617,37.3620789371229,-1.09608216684022));
#7707=CARTESIAN_POINT('Ctrl Pts',(1.97034563013915,37.5704122704562,-0.646824805365941));
#7708=CARTESIAN_POINT('Ctrl Pts',(2.00006370137914,37.7787456037895,-0.110909351770645));
#7709=CARTESIAN_POINT('Ctrl Pts',(2.02978177261915,37.9870789371229,0.425006101824736));
#7710=CARTESIAN_POINT('Ctrl Pts',(1.78756065046677,38.1954122704563,0.90398153453892));
#7711=CARTESIAN_POINT('Ctrl Pts',(1.5453395283144,38.4037456037895,1.38295696725319));
#7712=CARTESIAN_POINT('Ctrl Pts',(1.09608216684019,38.6120789371229,1.67665129869612));
#7713=CARTESIAN_POINT('Ctrl Pts',(0.646824805365943,38.8204122704562,1.97034563013916));
#7714=CARTESIAN_POINT('Ctrl Pts',(0.110909351770614,39.0287456037896,2.0000637013791));
#7715=CARTESIAN_POINT('Ctrl Pts',(-0.425006101824727,39.2370789371229,2.02978177261914));
#7716=CARTESIAN_POINT('Ctrl Pts',(-0.90398153453895,39.4454122704563,1.78756065046672));
#7717=CARTESIAN_POINT('Ctrl Pts',(-1.38295696725319,39.6537456037896,1.54533952831436));
#7718=CARTESIAN_POINT('Ctrl Pts',(-1.67665129869616,39.8620789371229,1.09608216684011));
#7719=CARTESIAN_POINT('Ctrl Pts',(-1.97034563013914,40.0704122704562,0.646824805365955));
#7720=CARTESIAN_POINT('Ctrl Pts',(-2.00006370137914,40.2787456037896,0.110909351770527));
#7721=CARTESIAN_POINT('',(-2.,-0.278745610073463,-0.11090935427092));
#7722=CARTESIAN_POINT('Origin',(-2.,-2.08166817117217E-14,-3.46944695195361E-14));
#7723=CARTESIAN_POINT('',(-2.,39.7212543899267,-0.110909354270961));
#7724=CARTESIAN_POINT('Ctrl Pts',(-2.,-0.278745610073463,-0.11090935427092));
#7725=CARTESIAN_POINT('Ctrl Pts',(-1.97028192809006,-0.0704122767402083,
-0.646807739133109));
#7726=CARTESIAN_POINT('Ctrl Pts',(-1.67659613043344,0.137921056593222,-1.0960503183159));
#7727=CARTESIAN_POINT('Ctrl Pts',(-1.38291033277683,0.346254389926512,-1.54529289749873));
#7728=CARTESIAN_POINT('Ctrl Pts',(-0.903949681684104,0.554587723259871,
-1.78750548470438));
#7729=CARTESIAN_POINT('Ctrl Pts',(-0.424989030591367,0.762921056593226,
-2.02971807190993));
#7730=CARTESIAN_POINT('Ctrl Pts',(0.110909354270878,0.971254389926561,-2.00000000000006));
#7731=CARTESIAN_POINT('Ctrl Pts',(0.646807739133123,1.17958772325984,-1.97028192809007));
#7732=CARTESIAN_POINT('Ctrl Pts',(1.09605031831591,1.38792105659322,-1.67659613043344));
#7733=CARTESIAN_POINT('Ctrl Pts',(1.54529289749868,1.59625438992652,-1.38291033277687));
#7734=CARTESIAN_POINT('Ctrl Pts',(1.78750548470428,1.80458772325989,-0.903949681684113));
#7735=CARTESIAN_POINT('Ctrl Pts',(2.02971807190996,2.01292105659317,-0.424989030591391));
#7736=CARTESIAN_POINT('Ctrl Pts',(2.,2.22125438992656,0.110909354270855));
#7737=CARTESIAN_POINT('Ctrl Pts',(1.97028192809007,2.42958772325984,0.646807739133102));
#7738=CARTESIAN_POINT('Ctrl Pts',(1.67659613043345,2.63792105659317,1.09605031831587));
#7739=CARTESIAN_POINT('Ctrl Pts',(1.38291033277683,2.8462543899265,1.54529289749866));
#7740=CARTESIAN_POINT('Ctrl Pts',(0.903949681684104,3.0545877232599,1.78750548470426));
#7741=CARTESIAN_POINT('Ctrl Pts',(0.424989030591383,3.26292105659317,2.02971807190993));
#7742=CARTESIAN_POINT('Ctrl Pts',(-0.11090935427085,3.47125438992654,1.99999999999995));
#7743=CARTESIAN_POINT('Ctrl Pts',(-0.646807739133109,3.67958772325983,1.97028192809007));
#7744=CARTESIAN_POINT('Ctrl Pts',(-1.0960503183159,3.88792105659323,1.67659613043343));
#7745=CARTESIAN_POINT('Ctrl Pts',(-1.54529289749868,4.09625438992648,1.38291033277681));
#7746=CARTESIAN_POINT('Ctrl Pts',(-1.78750548470431,4.30458772325989,0.903949681684051));
#7747=CARTESIAN_POINT('Ctrl Pts',(-2.02971807190994,4.51292105659318,0.424989030591333));
#7748=CARTESIAN_POINT('Ctrl Pts',(-2.,4.72125438992654,-0.110909354270966));
#7749=CARTESIAN_POINT('Ctrl Pts',(-1.97028192809006,4.92958772325984,-0.646807739133087));
#7750=CARTESIAN_POINT('Ctrl Pts',(-1.67659613043343,5.13792105659321,-1.09605031831595));
#7751=CARTESIAN_POINT('Ctrl Pts',(-1.38291033277683,5.34625438992653,-1.54529289749872));
#7752=CARTESIAN_POINT('Ctrl Pts',(-0.903949681684091,5.5545877232599,-1.78750548470436));
#7753=CARTESIAN_POINT('Ctrl Pts',(-0.424989030591382,5.76292105659322,-2.02971807190993));
#7754=CARTESIAN_POINT('Ctrl Pts',(0.110909354270865,5.97125438992659,-2.00000000000009));
#7755=CARTESIAN_POINT('Ctrl Pts',(0.646807739133111,6.17958772325983,-1.97028192809005));
#7756=CARTESIAN_POINT('Ctrl Pts',(1.0960503183159,6.38792105659326,-1.67659613043349));
#7757=CARTESIAN_POINT('Ctrl Pts',(1.54529289749868,6.5962543899265,-1.38291033277683));
#7758=CARTESIAN_POINT('Ctrl Pts',(1.7875054847043,6.80458772325989,-0.903949681684162));
#7759=CARTESIAN_POINT('Ctrl Pts',(2.02971807190991,7.01292105659322,-0.424989030591398));
#7760=CARTESIAN_POINT('Ctrl Pts',(2.,7.22125438992656,0.110909354270862));
#7761=CARTESIAN_POINT('Ctrl Pts',(1.97028192809006,7.42958772325989,0.646807739133109));
#7762=CARTESIAN_POINT('Ctrl Pts',(1.67659613043344,7.63792105659322,1.09605031831585));
#7763=CARTESIAN_POINT('Ctrl Pts',(1.38291033277683,7.84625438992656,1.54529289749869));
#7764=CARTESIAN_POINT('Ctrl Pts',(0.903949681684104,8.05458772325989,1.78750548470431));
#7765=CARTESIAN_POINT('Ctrl Pts',(0.424989030591398,8.26292105659318,2.02971807190991));
#7766=CARTESIAN_POINT('Ctrl Pts',(-0.110909354270878,8.47125438992655,1.99999999999995));
#7767=CARTESIAN_POINT('Ctrl Pts',(-0.646807739133123,8.67958772325983,1.97028192809004));
#7768=CARTESIAN_POINT('Ctrl Pts',(-1.0960503183159,8.88792105659324,1.67659613043339));
#7769=CARTESIAN_POINT('Ctrl Pts',(-1.54529289749868,9.0962543899265,1.38291033277683));
#7770=CARTESIAN_POINT('Ctrl Pts',(-1.78750548470431,9.3045877232599,0.903949681684085));
#7771=CARTESIAN_POINT('Ctrl Pts',(-2.02971807190993,9.51292105659317,0.424989030591355));
#7772=CARTESIAN_POINT('Ctrl Pts',(-2.,9.72125438992657,-0.110909354270924));
#7773=CARTESIAN_POINT('Ctrl Pts',(-1.97028192809007,9.92958772325984,-0.646807739133123));
#7774=CARTESIAN_POINT('Ctrl Pts',(-1.67659613043344,10.1379210565932,-1.09605031831599));
#7775=CARTESIAN_POINT('Ctrl Pts',(-1.38291033277681,10.3462543899265,-1.54529289749875));
#7776=CARTESIAN_POINT('Ctrl Pts',(-0.903949681684116,10.5545877232599,-1.78750548470438));
#7777=CARTESIAN_POINT('Ctrl Pts',(-0.424989030591382,10.7629210565932,-2.02971807190998));
#7778=CARTESIAN_POINT('Ctrl Pts',(0.110909354270878,10.9712543899266,-2.00000000000009));
#7779=CARTESIAN_POINT('Ctrl Pts',(0.646807739133123,11.1795877232599,-1.97028192809007));
#7780=CARTESIAN_POINT('Ctrl Pts',(1.09605031831591,11.3879210565932,-1.67659613043351));
#7781=CARTESIAN_POINT('Ctrl Pts',(1.54529289749868,11.5962543899266,-1.38291033277683));
#7782=CARTESIAN_POINT('Ctrl Pts',(1.78750548470431,11.8045877232599,-0.903949681684182));
#7783=CARTESIAN_POINT('Ctrl Pts',(2.02971807190994,12.0129210565932,-0.424989030591383));
#7784=CARTESIAN_POINT('Ctrl Pts',(2.,12.2212543899266,0.110909354270862));
#7785=CARTESIAN_POINT('Ctrl Pts',(1.97028192809007,12.4295877232599,0.646807739133051));
#7786=CARTESIAN_POINT('Ctrl Pts',(1.67659613043345,12.6379210565932,1.09605031831589));
#7787=CARTESIAN_POINT('Ctrl Pts',(1.38291033277683,12.8462543899266,1.54529289749867));
#7788=CARTESIAN_POINT('Ctrl Pts',(0.903949681684118,13.0545877232599,1.78750548470425));
#7789=CARTESIAN_POINT('Ctrl Pts',(0.424989030591382,13.2629210565932,2.02971807190993));
#7790=CARTESIAN_POINT('Ctrl Pts',(-0.110909354270864,13.4712543899266,1.99999999999997));
#7791=CARTESIAN_POINT('Ctrl Pts',(-0.646807739133109,13.6795877232599,1.97028192809006));
#7792=CARTESIAN_POINT('Ctrl Pts',(-1.0960503183159,13.8879210565932,1.67659613043339));
#7793=CARTESIAN_POINT('Ctrl Pts',(-1.54529289749868,14.0962543899266,1.38291033277683));
#7794=CARTESIAN_POINT('Ctrl Pts',(-1.7875054847043,14.3045877232599,0.903949681684092));
#7795=CARTESIAN_POINT('Ctrl Pts',(-2.02971807190994,14.5129210565932,0.424989030591326));
#7796=CARTESIAN_POINT('Ctrl Pts',(-2.,14.7212543899266,-0.110909354270938));
#7797=CARTESIAN_POINT('Ctrl Pts',(-1.97028192809006,14.9295877232599,-0.646807739133109));
#7798=CARTESIAN_POINT('Ctrl Pts',(-1.67659613043344,15.1379210565933,-1.09605031831595));
#7799=CARTESIAN_POINT('Ctrl Pts',(-1.38291033277683,15.3462543899265,-1.54529289749874));
#7800=CARTESIAN_POINT('Ctrl Pts',(-0.903949681684104,15.5545877232599,-1.78750548470439));
#7801=CARTESIAN_POINT('Ctrl Pts',(-0.424989030591382,15.7629210565932,-2.02971807190993));
#7802=CARTESIAN_POINT('Ctrl Pts',(0.110909354270852,15.9712543899266,-2.00000000000006));
#7803=CARTESIAN_POINT('Ctrl Pts',(0.646807739133109,16.1795877232599,-1.97028192809006));
#7804=CARTESIAN_POINT('Ctrl Pts',(1.0960503183159,16.3879210565933,-1.67659613043349));
#7805=CARTESIAN_POINT('Ctrl Pts',(1.5452928974987,16.5962543899265,-1.38291033277688));
#7806=CARTESIAN_POINT('Ctrl Pts',(1.78750548470431,16.8045877232599,-0.903949681684148));
#7807=CARTESIAN_POINT('Ctrl Pts',(2.02971807190994,17.0129210565932,-0.424989030591383));
#7808=CARTESIAN_POINT('Ctrl Pts',(2.,17.2212543899266,0.110909354270813));
#7809=CARTESIAN_POINT('Ctrl Pts',(1.97028192809007,17.4295877232599,0.646807739133109));
#7810=CARTESIAN_POINT('Ctrl Pts',(1.67659613043345,17.6379210565933,1.09605031831585));
#7811=CARTESIAN_POINT('Ctrl Pts',(1.38291033277684,17.8462543899265,1.54529289749865));
#7812=CARTESIAN_POINT('Ctrl Pts',(0.903949681684104,18.0545877232599,1.78750548470431));
#7813=CARTESIAN_POINT('Ctrl Pts',(0.424989030591369,18.2629210565932,2.02971807190994));
#7814=CARTESIAN_POINT('Ctrl Pts',(-0.110909354270865,18.4712543899266,2.));
#7815=CARTESIAN_POINT('Ctrl Pts',(-0.646807739133109,18.6795877232599,1.97028192809006));
#7816=CARTESIAN_POINT('Ctrl Pts',(-1.0960503183159,18.8879210565933,1.6765961304334));
#7817=CARTESIAN_POINT('Ctrl Pts',(-1.54529289749867,19.0962543899266,1.38291033277683));
#7818=CARTESIAN_POINT('Ctrl Pts',(-1.78750548470431,19.3045877232599,0.903949681684071));
#7819=CARTESIAN_POINT('Ctrl Pts',(-2.02971807190993,19.5129210565932,0.42498903059134));
#7820=CARTESIAN_POINT('Ctrl Pts',(-2.,19.7212543899266,-0.110909354270924));
#7821=CARTESIAN_POINT('Ctrl Pts',(-1.97028192809006,19.9295877232599,-0.646807739133152));
#7822=CARTESIAN_POINT('Ctrl Pts',(-1.67659613043345,20.1379210565933,-1.09605031831597));
#7823=CARTESIAN_POINT('Ctrl Pts',(-1.38291033277683,20.3462543899266,-1.54529289749875));
#7824=CARTESIAN_POINT('Ctrl Pts',(-0.903949681684103,20.5545877232599,-1.78750548470438));
#7825=CARTESIAN_POINT('Ctrl Pts',(-0.424989030591367,20.7629210565932,-2.02971807190997));
#7826=CARTESIAN_POINT('Ctrl Pts',(0.110909354270864,20.9712543899266,-2.0000000000001));
#7827=CARTESIAN_POINT('Ctrl Pts',(0.646807739133111,21.1795877232599,-1.97028192809011));
#7828=CARTESIAN_POINT('Ctrl Pts',(1.0960503183159,21.3879210565933,-1.67659613043352));
#7829=CARTESIAN_POINT('Ctrl Pts',(1.54529289749868,21.5962543899266,-1.38291033277683));
#7830=CARTESIAN_POINT('Ctrl Pts',(1.78750548470431,21.8045877232599,-0.90394968168419));
#7831=CARTESIAN_POINT('Ctrl Pts',(2.02971807190991,22.0129210565932,-0.424989030591391));
#7832=CARTESIAN_POINT('Ctrl Pts',(2.,22.2212543899266,0.110909354270855));
#7833=CARTESIAN_POINT('Ctrl Pts',(1.97028192809009,22.4295877232599,0.646807739133087));
#7834=CARTESIAN_POINT('Ctrl Pts',(1.67659613043345,22.6379210565933,1.09605031831588));
#7835=CARTESIAN_POINT('Ctrl Pts',(1.38291033277683,22.8462543899266,1.54529289749862));
#7836=CARTESIAN_POINT('Ctrl Pts',(0.903949681684118,23.0545877232599,1.78750548470426));
#7837=CARTESIAN_POINT('Ctrl Pts',(0.424989030591383,23.2629210565932,2.02971807190993));
#7838=CARTESIAN_POINT('Ctrl Pts',(-0.110909354270864,23.4712543899266,1.99999999999997));
#7839=CARTESIAN_POINT('Ctrl Pts',(-0.646807739133109,23.6795877232599,1.97028192809003));
#7840=CARTESIAN_POINT('Ctrl Pts',(-1.09605031831588,23.8879210565933,1.67659613043339));
#7841=CARTESIAN_POINT('Ctrl Pts',(-1.54529289749869,24.0962543899266,1.38291033277683));
#7842=CARTESIAN_POINT('Ctrl Pts',(-1.78750548470431,24.3045877232599,0.903949681684092));
#7843=CARTESIAN_POINT('Ctrl Pts',(-2.02971807190995,24.5129210565932,0.424989030591319));
#7844=CARTESIAN_POINT('Ctrl Pts',(-2.,24.7212543899266,-0.110909354270938));
#7845=CARTESIAN_POINT('Ctrl Pts',(-1.97028192809005,24.9295877232599,-0.646807739133109));
#7846=CARTESIAN_POINT('Ctrl Pts',(-1.67659613043344,25.1379210565933,-1.09605031831594));
#7847=CARTESIAN_POINT('Ctrl Pts',(-1.38291033277683,25.3462543899266,-1.54529289749872));
#7848=CARTESIAN_POINT('Ctrl Pts',(-0.903949681684104,25.55458772326,-1.7875054847044));
#7849=CARTESIAN_POINT('Ctrl Pts',(-0.424989030591382,25.7629210565933,-2.02971807190993));
#7850=CARTESIAN_POINT('Ctrl Pts',(0.110909354270864,25.9712543899266,-2.00000000000006));
#7851=CARTESIAN_POINT('Ctrl Pts',(0.646807739133109,26.1795877232599,-1.97028192809006));
#7852=CARTESIAN_POINT('Ctrl Pts',(1.0960503183159,26.3879210565933,-1.67659613043348));
#7853=CARTESIAN_POINT('Ctrl Pts',(1.5452928974987,26.5962543899266,-1.38291033277687));
#7854=CARTESIAN_POINT('Ctrl Pts',(1.78750548470431,26.80458772326,-0.903949681684155));
#7855=CARTESIAN_POINT('Ctrl Pts',(2.02971807190994,27.0129210565933,-0.424989030591383));
#7856=CARTESIAN_POINT('Ctrl Pts',(2.00000000000003,27.2212543899266,0.11090935427082));
#7857=CARTESIAN_POINT('Ctrl Pts',(1.97028192809007,27.4295877232599,0.646807739133109));
#7858=CARTESIAN_POINT('Ctrl Pts',(1.67659613043345,27.6379210565933,1.09605031831587));
#7859=CARTESIAN_POINT('Ctrl Pts',(1.38291033277684,27.8462543899266,1.54529289749868));
#7860=CARTESIAN_POINT('Ctrl Pts',(0.903949681684103,28.0545877232599,1.78750548470431));
#7861=CARTESIAN_POINT('Ctrl Pts',(0.424989030591382,28.2629210565932,2.02971807190993));
#7862=CARTESIAN_POINT('Ctrl Pts',(-0.110909354270852,28.4712543899266,1.99999999999998));
#7863=CARTESIAN_POINT('Ctrl Pts',(-0.646807739133109,28.6795877232599,1.97028192809006));
#7864=CARTESIAN_POINT('Ctrl Pts',(-1.0960503183159,28.8879210565933,1.67659613043341));
#7865=CARTESIAN_POINT('Ctrl Pts',(-1.54529289749868,29.0962543899266,1.38291033277683));
#7866=CARTESIAN_POINT('Ctrl Pts',(-1.78750548470432,29.30458772326,0.903949681684071));
#7867=CARTESIAN_POINT('Ctrl Pts',(-2.02971807190994,29.5129210565933,0.42498903059134));
#7868=CARTESIAN_POINT('Ctrl Pts',(-2.,29.7212543899266,-0.110909354270917));
#7869=CARTESIAN_POINT('Ctrl Pts',(-1.97028192809006,29.9295877232599,-0.646807739133087));
#7870=CARTESIAN_POINT('Ctrl Pts',(-1.67659613043345,30.1379210565933,-1.09605031831597));
#7871=CARTESIAN_POINT('Ctrl Pts',(-1.38291033277683,30.3462543899266,-1.54529289749872));
#7872=CARTESIAN_POINT('Ctrl Pts',(-0.903949681684103,30.55458772326,-1.78750548470437));
#7873=CARTESIAN_POINT('Ctrl Pts',(-0.424989030591367,30.7629210565933,-2.02971807190996));
#7874=CARTESIAN_POINT('Ctrl Pts',(0.110909354270865,30.9712543899266,-2.00000000000009));
#7875=CARTESIAN_POINT('Ctrl Pts',(0.646807739133123,31.1795877232599,-1.97028192809004));
#7876=CARTESIAN_POINT('Ctrl Pts',(1.0960503183159,31.3879210565933,-1.67659613043352));
#7877=CARTESIAN_POINT('Ctrl Pts',(1.54529289749868,31.5962543899266,-1.38291033277685));
#7878=CARTESIAN_POINT('Ctrl Pts',(1.78750548470431,31.80458772326,-0.903949681684169));
#7879=CARTESIAN_POINT('Ctrl Pts',(2.02971807190994,32.0129210565933,-0.424989030591419));
#7880=CARTESIAN_POINT('Ctrl Pts',(2.,32.2212543899266,0.110909354270869));
#7881=CARTESIAN_POINT('Ctrl Pts',(1.97028192809004,32.4295877232599,0.646807739133087));
#7882=CARTESIAN_POINT('Ctrl Pts',(1.67659613043345,32.6379210565933,1.09605031831587));
#7883=CARTESIAN_POINT('Ctrl Pts',(1.38291033277683,32.8462543899266,1.54529289749868));
#7884=CARTESIAN_POINT('Ctrl Pts',(0.903949681684104,33.0545877232599,1.78750548470431));
#7885=CARTESIAN_POINT('Ctrl Pts',(0.424989030591383,33.2629210565932,2.02971807190993));
#7886=CARTESIAN_POINT('Ctrl Pts',(-0.110909354270864,33.4712543899267,1.99999999999997));
#7887=CARTESIAN_POINT('Ctrl Pts',(-0.646807739133109,33.6795877232599,1.97028192809004));
#7888=CARTESIAN_POINT('Ctrl Pts',(-1.09605031831588,33.8879210565934,1.6765961304334));
#7889=CARTESIAN_POINT('Ctrl Pts',(-1.54529289749868,34.0962543899266,1.38291033277683));
#7890=CARTESIAN_POINT('Ctrl Pts',(-1.78750548470431,34.30458772326,0.903949681684037));
#7891=CARTESIAN_POINT('Ctrl Pts',(-2.02971807190994,34.5129210565932,0.424989030591383));
#7892=CARTESIAN_POINT('Ctrl Pts',(-2.,34.7212543899267,-0.110909354270938));
#7893=CARTESIAN_POINT('Ctrl Pts',(-1.97028192809006,34.9295877232599,-0.646807739133123));
#7894=CARTESIAN_POINT('Ctrl Pts',(-1.67659613043344,35.1379210565933,-1.09605031831594));
#7895=CARTESIAN_POINT('Ctrl Pts',(-1.38291033277683,35.3462543899267,-1.54529289749875));
#7896=CARTESIAN_POINT('Ctrl Pts',(-0.903949681684103,35.55458772326,-1.78750548470439));
#7897=CARTESIAN_POINT('Ctrl Pts',(-0.424989030591382,35.7629210565932,-2.02971807190993));
#7898=CARTESIAN_POINT('Ctrl Pts',(0.110909354270864,35.9712543899267,-2.00000000000003));
#7899=CARTESIAN_POINT('Ctrl Pts',(0.646807739133111,36.1795877232599,-1.97028192809006));
#7900=CARTESIAN_POINT('Ctrl Pts',(1.0960503183159,36.3879210565933,-1.67659613043348));
#7901=CARTESIAN_POINT('Ctrl Pts',(1.54529289749869,36.5962543899266,-1.38291033277682));
#7902=CARTESIAN_POINT('Ctrl Pts',(1.78750548470431,36.80458772326,-0.903949681684127));
#7903=CARTESIAN_POINT('Ctrl Pts',(2.02971807190994,37.0129210565932,-0.424989030591383));
#7904=CARTESIAN_POINT('Ctrl Pts',(2.,37.2212543899267,0.110909354270834));
#7905=CARTESIAN_POINT('Ctrl Pts',(1.97028192809006,37.4295877232599,0.646807739133109));
#7906=CARTESIAN_POINT('Ctrl Pts',(1.67659613043345,37.6379210565933,1.09605031831588));
#7907=CARTESIAN_POINT('Ctrl Pts',(1.38291033277681,37.8462543899266,1.54529289749865));
#7908=CARTESIAN_POINT('Ctrl Pts',(0.903949681684104,38.0545877232599,1.78750548470431));
#7909=CARTESIAN_POINT('Ctrl Pts',(0.424989030591383,38.2629210565933,2.02971807190991));
#7910=CARTESIAN_POINT('Ctrl Pts',(-0.11090935427085,38.4712543899266,1.99999999999995));
#7911=CARTESIAN_POINT('Ctrl Pts',(-0.646807739133111,38.67958772326,1.97028192809006));
#7912=CARTESIAN_POINT('Ctrl Pts',(-1.0960503183159,38.8879210565933,1.67659613043344));
#7913=CARTESIAN_POINT('Ctrl Pts',(-1.54529289749868,39.0962543899266,1.38291033277682));
#7914=CARTESIAN_POINT('Ctrl Pts',(-1.78750548470431,39.30458772326,0.903949681684064));
#7915=CARTESIAN_POINT('Ctrl Pts',(-2.02971807190993,39.5129210565932,0.424989030591368));
#7916=CARTESIAN_POINT('Ctrl Pts',(-2.,39.7212543899267,-0.110909354270961));
#7917=CARTESIAN_POINT('',(-1.99999999999999,40.2787456100736,0.110909354270809));
#7918=CARTESIAN_POINT('Origin',(-1.99999999999999,40.0000000000001,-7.63278329429795E-14));
#7919=CARTESIAN_POINT('',(-2.00308415717522,0.327811454287795,-0.014474292615955));
#7920=CARTESIAN_POINT('Ctrl Pts',(-2.00308415717522,0.327811454287795,-0.014474292615955));
#7921=CARTESIAN_POINT('Ctrl Pts',(-2.00266941950797,0.3499571598645,-0.0706947258144284));
#7922=CARTESIAN_POINT('Ctrl Pts',(-1.99988284484963,0.37238501496934,-0.127135039387294));
#7923=CARTESIAN_POINT('Ctrl Pts',(-1.99469178463351,0.394978788957426,-0.183493113344122));
#7924=CARTESIAN_POINT('Ctrl Pts',(-1.98950037298493,0.417574092533932,-0.239855002717413));
#7925=CARTESIAN_POINT('Ctrl Pts',(-1.98190404906885,0.440335059872151,-0.296133914952173));
#7926=CARTESIAN_POINT('Ctrl Pts',(-1.97192179180133,0.463139554738375,-0.352023517509166));
#7927=CARTESIAN_POINT('Ctrl Pts',(-1.96194535902849,0.485930743530098,-0.407880509336571));
#7928=CARTESIAN_POINT('Ctrl Pts',(-1.94958586765235,0.508765113065188,-0.463347912701799));
#7929=CARTESIAN_POINT('Ctrl Pts',(-1.93491390431575,0.531519187675631,-0.518126779296725));
#7930=CARTESIAN_POINT('Ctrl Pts',(-1.92022340561799,0.554302007927083,-0.572974849041457));
#7931=CARTESIAN_POINT('Ctrl Pts',(-1.90321484710063,0.577004036127603,-0.627131948034054));
#7932=CARTESIAN_POINT('Ctrl Pts',(-1.88400825633397,0.59950422083275,-0.680315621374878));
#7933=CARTESIAN_POINT('Ctrl Pts',(-1.86482690562689,0.621974837250142,-0.733429404171343));
#7934=CARTESIAN_POINT('Ctrl Pts',(-1.84345373271557,0.64424387424164,-0.785571733351559));
#7935=CARTESIAN_POINT('Ctrl Pts',(-1.82005202898671,0.666197857568301,-0.836488448064752));
#7936=CARTESIAN_POINT('Ctrl Pts',(-1.80960152082968,0.676001856648568,-0.859226345638543));
#7937=CARTESIAN_POINT('Ctrl Pts',(-1.79874701482939,0.68574314488471,-0.88172023997714));
#7938=CARTESIAN_POINT('Ctrl Pts',(-1.78750548470434,0.695412276740075,-0.903949681684082));
#7939=CARTESIAN_POINT('Ctrl Pts',(-1.76228706012996,0.717103298307556,-0.953817581585667));
#7940=CARTESIAN_POINT('Ctrl Pts',(-1.73483868812781,0.739157960797294,-1.00290422620941));
#7941=CARTESIAN_POINT('Ctrl Pts',(-1.70524671607301,0.761466638112126,-1.05092079729495));
#7942=CARTESIAN_POINT('Ctrl Pts',(-1.67569471956003,0.783745178825665,-1.09887250320548));
#7943=CARTESIAN_POINT('Ctrl Pts',(-1.644005063612,0.806276796082526,-1.14575631858766));
#7944=CARTESIAN_POINT('Ctrl Pts',(-1.610312845326,0.828943478358563,-1.19129904937546));
#7945=CARTESIAN_POINT('Ctrl Pts',(-1.57620686948493,0.851888519006865,-1.23740106803152));
#7946=CARTESIAN_POINT('Ctrl Pts',(-1.54004908312197,0.874971676226894,-1.28212811955073));
#7947=CARTESIAN_POINT('Ctrl Pts',(-1.50202718276504,0.898065543699821,-1.32522270849081));
#7948=CARTESIAN_POINT('Ctrl Pts',(-1.46447392216126,0.920874767210976,-1.36778613414519));
#7949=CARTESIAN_POINT('Ctrl Pts',(-1.42510278850771,0.943694135502599,-1.40875659069773));
#7950=CARTESIAN_POINT('Ctrl Pts',(-1.38413434133606,0.966400507514448,-1.4479202360624));
#7951=CARTESIAN_POINT('Ctrl Pts',(-1.3423990056442,0.989531920191343,-1.48781698585533));
#7952=CARTESIAN_POINT('Ctrl Pts',(-1.29900653939395,1.01254574679517,-1.52583806568238));
#7953=CARTESIAN_POINT('Ctrl Pts',(-1.25422343600175,1.03531613020345,-1.56180167033104));
#7954=CARTESIAN_POINT('Ctrl Pts',(-1.20944033260954,1.05808651361172,-1.5977652749797));
#7955=CARTESIAN_POINT('Ctrl Pts',(-1.16326733827024,1.08061317258821,-1.63167113305563));
#7956=CARTESIAN_POINT('Ctrl Pts',(-1.11599400238479,1.10277908871816,-1.66338758908019));
#7957=CARTESIAN_POINT('Ctrl Pts',(-1.10936742882085,1.10588621181613,-1.66783346591748));
#7958=CARTESIAN_POINT('Ctrl Pts',(-1.1027192606465,1.1089862646405,-1.67223640644771));
#7959=CARTESIAN_POINT('Ctrl Pts',(-1.09605031831594,1.11207894340675,-1.67659613043344));
#7960=CARTESIAN_POINT('Ctrl Pts',(-1.04927657204218,1.13376996497337,-1.70717378629317));
#7961=CARTESIAN_POINT('Ctrl Pts',(-1.00096226228592,1.15582462746222,-1.73595988152172));
#7962=CARTESIAN_POINT('Ctrl Pts',(-0.951326577197707,1.17813330477615,-1.76274746585609));
#7963=CARTESIAN_POINT('Ctrl Pts',(-0.901757944525814,1.20041184549145,-1.78949886307521));
#7964=CARTESIAN_POINT('Ctrl Pts',(-0.850871989742473,1.22294346275011,-1.81425661025049));
#7965=CARTESIAN_POINT('Ctrl Pts',(-0.79892230739882,1.24561014502797,-1.83685166292907));
#7966=CARTESIAN_POINT('Ctrl Pts',(-0.746334656571898,1.26855518567611,-1.85972419433008));
#7967=CARTESIAN_POINT('Ctrl Pts',(-0.692657569277719,1.29163834289596,-1.88038006400027));
#7968=CARTESIAN_POINT('Ctrl Pts',(-0.638182343198804,1.31473221036871,-1.89869012260928));
#7969=CARTESIAN_POINT('Ctrl Pts',(-0.58437855269953,1.33754143387742,-1.91677450019409));
#7970=CARTESIAN_POINT('Ctrl Pts',(-0.529796922509381,1.36036080216659,-1.93257038954486));
#7971=CARTESIAN_POINT('Ctrl Pts',(-0.474735383828777,1.38306717417602,-1.94600287774858));
#7972=CARTESIAN_POINT('Ctrl Pts',(-0.418643147985475,1.40619858685387,-1.95968680875268));
#7973=CARTESIAN_POINT('Ctrl Pts',(-0.3620536299641,1.42921241345865,-1.97091779663782));
#7974=CARTESIAN_POINT('Ctrl Pts',(-0.305288522439514,1.45198279686787,-1.97967164017963));
#7975=CARTESIAN_POINT('Ctrl Pts',(-0.248523414914927,1.47475318027709,-1.98842548372145));
#7976=CARTESIAN_POINT('Ctrl Pts',(-0.191583499807998,1.49727983925449,-1.99470232098299));
#7977=CARTESIAN_POINT('Ctrl Pts',(-0.134785361994971,1.51944575538534,-1.99853290967568));
#7978=CARTESIAN_POINT('Ctrl Pts',(-0.126823642530318,1.52255287848314,-1.99906986517686));
#7979=CARTESIAN_POINT('Ctrl Pts',(-0.118864689737994,1.52565293130735,-1.99955883944018));
#7980=CARTESIAN_POINT('Ctrl Pts',(-0.110909354270907,1.52874561007343,-2.00000000000001));
#7981=CARTESIAN_POINT('Ctrl Pts',(-0.0551132738209439,1.5504366316466,-2.0030941536268));
#7982=CARTESIAN_POINT('Ctrl Pts',(0.00112119342568086,1.57249129414221,
-2.00386648849188));
#7983=CARTESIAN_POINT('Ctrl Pts',(0.0575007498306207,1.59479997146302,-2.00224737448543));
#7984=CARTESIAN_POINT('Ctrl Pts',(0.113804143542876,1.61707851216972,-2.00063044772718));
#7985=CARTESIAN_POINT('Ctrl Pts',(0.170251546646483,1.63961012941955,-1.99662830833083));
#7986=CARTESIAN_POINT('Ctrl Pts',(0.226538817591831,1.66227681168847,-1.99022135678145));
#7987=CARTESIAN_POINT('Ctrl Pts',(0.283517324835077,1.68522185233709,-1.98373572461041));
#7988=CARTESIAN_POINT('Ctrl Pts',(0.34033098086939,1.70830500955743,-1.97478568883516));
#7989=CARTESIAN_POINT('Ctrl Pts',(0.396662939836441,1.73139887703068,-1.96340505169596));
#7990=CARTESIAN_POINT('Ctrl Pts',(0.452300578026043,1.75420810054139,-1.95216468684573));
#7991=CARTESIAN_POINT('Ctrl Pts',(0.507467601030938,1.77702746883257,-1.93855351320271));
#7992=CARTESIAN_POINT('Ctrl Pts',(0.561868536406385,1.79973384084398,-1.92265561988137));
#7993=CARTESIAN_POINT('Ctrl Pts',(0.617287803103204,1.82286525352159,-1.90646013383298));
#7994=CARTESIAN_POINT('Ctrl Pts',(0.671911257239619,1.84587908012614,-1.88789169564054));
#7995=CARTESIAN_POINT('Ctrl Pts',(0.725448204174811,1.86864946353513,-1.86709019276638));
#7996=CARTESIAN_POINT('Ctrl Pts',(0.778985151110002,1.89141984694411,-1.84628868989223));
#7997=CARTESIAN_POINT('Ctrl Pts',(0.831434982712155,1.91394650592129,-1.82325463286289));
#7998=CARTESIAN_POINT('Ctrl Pts',(0.882538907291713,1.93611242205192,-1.79817295107595));
#7999=CARTESIAN_POINT('Ctrl Pts',(0.889702436356562,1.93921954514975,-1.79465710844832));
#8000=CARTESIAN_POINT('Ctrl Pts',(0.896839578793958,1.94231959797399,-1.79110109618596));
#8001=CARTESIAN_POINT('Ctrl Pts',(0.903949681684062,1.94541227674011,-1.78750548470435));
#8002=CARTESIAN_POINT('Ctrl Pts',(0.953817581594439,1.96710329831142,-1.76228706012554));
#8003=CARTESIAN_POINT('Ctrl Pts',(1.00290422622669,1.98915796080511,-1.73483868811816));
#8004=CARTESIAN_POINT('Ctrl Pts',(1.0509207973203,2.01146663812396,-1.70524671605739));
#8005=CARTESIAN_POINT('Ctrl Pts',(1.09887250322638,2.0337451788357,-1.67569471954618));
#8006=CARTESIAN_POINT('Ctrl Pts',(1.14575631860424,2.05627679609069,-1.6440050636003));
#8007=CARTESIAN_POINT('Ctrl Pts',(1.19129904938792,2.07894347836483,-1.6103128453168));
#8008=CARTESIAN_POINT('Ctrl Pts',(1.23740106804277,2.10188851901268,-1.57620686947607));
#8009=CARTESIAN_POINT('Ctrl Pts',(1.28212811956079,2.12497167623223,-1.54004908311355));
#8010=CARTESIAN_POINT('Ctrl Pts',(1.32522270849975,2.14806554370468,-1.50202718275716));
#8011=CARTESIAN_POINT('Ctrl Pts',(1.36778613414331,2.17087476721016,-1.46447392216248));
#8012=CARTESIAN_POINT('Ctrl Pts',(1.40875659068581,2.19369413549609,-1.42510278851892));
#8013=CARTESIAN_POINT('Ctrl Pts',(1.44792023604139,2.21640050750233,-1.38413434135804));
#8014=CARTESIAN_POINT('Ctrl Pts',(1.4878169858386,2.23953192018137,-1.34239900566296));
#8015=CARTESIAN_POINT('Ctrl Pts',(1.52583806566963,2.26254574678733,-1.29900653940915));
#8016=CARTESIAN_POINT('Ctrl Pts',(1.56180167032191,2.28531613019772,-1.2542234360131));
#8017=CARTESIAN_POINT('Ctrl Pts',(1.59776527497418,2.3080865136081,-1.20944033261705));
#8018=CARTESIAN_POINT('Ctrl Pts',(1.63167113305336,2.33061317258665,-1.16326733827364));
#8019=CARTESIAN_POINT('Ctrl Pts',(1.66338758908079,2.35277908871862,-1.11599400238388));
#8020=CARTESIAN_POINT('Ctrl Pts',(1.66783346591787,2.35588621181643,-1.10936742882024));
#8021=CARTESIAN_POINT('Ctrl Pts',(1.67223640644789,2.35898626464066,-1.10271926064619));
#8022=CARTESIAN_POINT('Ctrl Pts',(1.67659613043342,2.36207894340677,-1.09605031831594));
#8023=CARTESIAN_POINT('Ctrl Pts',(1.70717378629795,2.38376996497678,-1.04927657203487));
#8024=CARTESIAN_POINT('Ctrl Pts',(1.73595988153072,2.40582462746913,-1.00096226227081));
#8025=CARTESIAN_POINT('Ctrl Pts',(1.76274746586867,2.42813330478662,-0.951326577174423));
#8026=CARTESIAN_POINT('Ctrl Pts',(1.78949886307852,2.4504118454948,-0.901757944518151));
#8027=CARTESIAN_POINT('Ctrl Pts',(1.81425661024578,2.47294346274615,-0.850871989751322));
#8028=CARTESIAN_POINT('Ctrl Pts',(1.83685166291778,2.49561014501663,-0.79892230742483));
#8029=CARTESIAN_POINT('Ctrl Pts',(1.85972419432044,2.51855518566565,-0.746334656596121));
#8030=CARTESIAN_POINT('Ctrl Pts',(1.88038006399214,2.54163834288643,-0.692657569300023));
#8031=CARTESIAN_POINT('Ctrl Pts',(1.89869012260248,2.56473221036011,-0.638182343219085));
#8032=CARTESIAN_POINT('Ctrl Pts',(1.9167745001887,2.58754143386987,-0.584378552717512));
#8033=CARTESIAN_POINT('Ctrl Pts',(1.93257038954068,2.61036080216012,-0.529796922524956));
#8034=CARTESIAN_POINT('Ctrl Pts',(1.94600287774539,2.63306717417062,-0.474735383841874));
#8035=CARTESIAN_POINT('Ctrl Pts',(1.95968680875038,2.65619858684937,-0.418643147996515));
#8036=CARTESIAN_POINT('Ctrl Pts',(1.97091779663624,2.67921241345505,-0.362053629973022));
#8037=CARTESIAN_POINT('Ctrl Pts',(1.97967164017859,2.70198279686515,-0.305288522446292));
#8038=CARTESIAN_POINT('Ctrl Pts',(1.98842548372093,2.72475318027525,-0.248523414919561));
#8039=CARTESIAN_POINT('Ctrl Pts',(1.99470232098281,2.74727983925353,-0.19158349981046));
#8040=CARTESIAN_POINT('Ctrl Pts',(1.99853290967565,2.76944575538522,-0.134785361995276));
#8041=CARTESIAN_POINT('Ctrl Pts',(1.99906986517684,2.77255287848306,-0.126823642530526));
#8042=CARTESIAN_POINT('Ctrl Pts',(1.99955883944017,2.77565293130731,-0.118864689738103));
#8043=CARTESIAN_POINT('Ctrl Pts',(2.00000000000001,2.77874561007344,-0.110909354270919));
#8044=CARTESIAN_POINT('Ctrl Pts',(2.00309415362589,2.80043663164038,-0.0551132738369698));
#8045=CARTESIAN_POINT('Ctrl Pts',(2.00386648849142,2.82249129412957,0.00112119339338623));
#8046=CARTESIAN_POINT('Ctrl Pts',(2.0022473744868,2.84479997144383,0.0575007497820639));
#8047=CARTESIAN_POINT('Ctrl Pts',(2.00063044772948,2.86707851215629,0.113804143509145));
#8048=CARTESIAN_POINT('Ctrl Pts',(1.99662830833282,2.88961012941204,0.170251546627733));
#8049=CARTESIAN_POINT('Ctrl Pts',(1.99022135678185,2.91227681168697,0.226538817587992));
#8050=CARTESIAN_POINT('Ctrl Pts',(1.98373572461087,2.93522185233572,0.2835173248316));
#8051=CARTESIAN_POINT('Ctrl Pts',(1.97478568883566,2.95830500955621,0.340330980866278));
#8052=CARTESIAN_POINT('Ctrl Pts',(1.96340505169648,2.9813988770296,0.396662939833696));
#8053=CARTESIAN_POINT('Ctrl Pts',(1.9521646868472,3.00420810053854,0.452300578019002));
#8054=CARTESIAN_POINT('Ctrl Pts',(1.9385535132055,3.02702746882794,0.507467601019676));
#8055=CARTESIAN_POINT('Ctrl Pts',(1.92265561988582,3.04973384083762,0.561868536391049));
#8056=CARTESIAN_POINT('Ctrl Pts',(1.90646013383709,3.07286525351635,0.61728780309064));
#8057=CARTESIAN_POINT('Ctrl Pts',(1.8878916956441,3.095879080122,0.671911257229776));
#8058=CARTESIAN_POINT('Ctrl Pts',(1.86709019276915,3.11864946353209,0.725448204167599));
#8059=CARTESIAN_POINT('Ctrl Pts',(1.84628868989421,3.14141984694217,0.778985151105422));
#8060=CARTESIAN_POINT('Ctrl Pts',(1.82325463286388,3.16394650592043,0.831434982710117));
#8061=CARTESIAN_POINT('Ctrl Pts',(1.79817295107574,3.1861124220521,0.882538907292086));
#8062=CARTESIAN_POINT('Ctrl Pts',(1.79465710844817,3.18921954514987,0.8897024363568));
#8063=CARTESIAN_POINT('Ctrl Pts',(1.79110109618588,3.19231959797405,0.896839578794061));
#8064=CARTESIAN_POINT('Ctrl Pts',(1.78750548470433,3.1954122767401,0.903949681684033));
#8065=CARTESIAN_POINT('Ctrl Pts',(1.76228706012363,3.21710329831304,0.953817581598165));
#8066=CARTESIAN_POINT('Ctrl Pts',(1.73483868811402,3.23915796080841,1.00290422623404));
#8067=CARTESIAN_POINT('Ctrl Pts',(1.70524671605071,3.26146663812897,1.0509207973311));
#8068=CARTESIAN_POINT('Ctrl Pts',(1.67569471954924,3.28374517883316,1.0988725032207));
#8069=CARTESIAN_POINT('Ctrl Pts',(1.64400506361456,3.30627679608043,1.14575631858279));
#8070=CARTESIAN_POINT('Ctrl Pts',(1.61031284534359,3.32894347834677,1.19129904935168));
#8071=CARTESIAN_POINT('Ctrl Pts',(1.57620686950167,3.35188851899607,1.2374010680103));
#8072=CARTESIAN_POINT('Ctrl Pts',(1.54004908313765,3.37497167621712,1.28212811953198));
#8073=CARTESIAN_POINT('Ctrl Pts',(1.50202718277948,3.39806554369109,1.32522270847443));
#8074=CARTESIAN_POINT('Ctrl Pts',(1.46447392218186,3.42087476719878,1.36778613412276));
#8075=CARTESIAN_POINT('Ctrl Pts',(1.42510278853499,3.44369413548695,1.40875659066976));
#8076=CARTESIAN_POINT('Ctrl Pts',(1.38413434137046,3.46640050749542,1.4479202360295));
#8077=CARTESIAN_POINT('Ctrl Pts',(1.34239900567359,3.48953192017566,1.48781698582912));
#8078=CARTESIAN_POINT('Ctrl Pts',(1.29900653941778,3.51254574678283,1.52583806566237));
#8079=CARTESIAN_POINT('Ctrl Pts',(1.25422343601959,3.5353161301944,1.56180167031668));
#8080=CARTESIAN_POINT('Ctrl Pts',(1.2094403326214,3.55808651360597,1.59776527497099));
#8081=CARTESIAN_POINT('Ctrl Pts',(1.16326733827567,3.5806131725857,1.63167113305201));
#8082=CARTESIAN_POINT('Ctrl Pts',(1.11599400238349,3.60277908871879,1.66338758908104));
#8083=CARTESIAN_POINT('Ctrl Pts',(1.10936742881998,3.60588621181655,1.66783346591803));
#8084=CARTESIAN_POINT('Ctrl Pts',(1.10271926064606,3.60898626464072,1.67223640644796));
#8085=CARTESIAN_POINT('Ctrl Pts',(1.09605031831594,3.61207894340676,1.67659613043341));
#8086=CARTESIAN_POINT('Ctrl Pts',(1.04927657204018,3.63376996497431,1.70717378629447));
#8087=CARTESIAN_POINT('Ctrl Pts',(1.00096226228176,3.65582462746412,1.73595988152418));
#8088=CARTESIAN_POINT('Ctrl Pts',(0.951326577191293,3.67813330477903,1.76274746585954));
#8089=CARTESIAN_POINT('Ctrl Pts',(0.901757944520491,3.70041184549381,1.78949886307784));
#8090=CARTESIAN_POINT('Ctrl Pts',(0.850871989738323,3.72294346275193,1.81425661025238));
#8091=CARTESIAN_POINT('Ctrl Pts',(0.798922307395897,3.74561014502924,1.83685166293033));
#8092=CARTESIAN_POINT('Ctrl Pts',(0.746334656569164,3.76855518567727,1.85972419433115));
#8093=CARTESIAN_POINT('Ctrl Pts',(0.692657569275196,3.79163834289702,1.88038006400118));
#8094=CARTESIAN_POINT('Ctrl Pts',(0.638182343196498,3.81473221036967,1.89869012261004));
#8095=CARTESIAN_POINT('Ctrl Pts',(0.584378552698208,3.83754143387795,1.91677450019444));
#8096=CARTESIAN_POINT('Ctrl Pts',(0.529796922509088,3.86036080216669,1.93257038954489));
#8097=CARTESIAN_POINT('Ctrl Pts',(0.474735383829518,3.88306717417569,1.94600287774836));
#8098=CARTESIAN_POINT('Ctrl Pts',(0.418643147986074,3.90619858685361,1.95968680875251));
#8099=CARTESIAN_POINT('Ctrl Pts',(0.362053629964559,3.92921241345845,1.9709177966377));
#8100=CARTESIAN_POINT('Ctrl Pts',(0.305288522439826,3.95198279686773,1.97967164017955));
#8101=CARTESIAN_POINT('Ctrl Pts',(0.248523414915094,3.97475318027701,1.9884254837214));
#8102=CARTESIAN_POINT('Ctrl Pts',(0.191583499808025,3.99727983925448,1.99470232098295));
#8103=CARTESIAN_POINT('Ctrl Pts',(0.134785361994851,4.01944575538539,1.99853290967564));
#8104=CARTESIAN_POINT('Ctrl Pts',(0.126823642530245,4.02255287848317,1.99906986517682));
#8105=CARTESIAN_POINT('Ctrl Pts',(0.118864689737964,4.02565293130737,1.99955883944014));
#8106=CARTESIAN_POINT('Ctrl Pts',(0.110909354270922,4.02874561007343,1.99999999999997));
#8107=CARTESIAN_POINT('Ctrl Pts',(0.0551132738242976,4.0504366316453,2.00309415362657));
#8108=CARTESIAN_POINT('Ctrl Pts',(-0.00112119341893398,4.07249129413957,
2.00386648849175));
#8109=CARTESIAN_POINT('Ctrl Pts',(-0.0575007498204855,4.09479997145902,
2.00224737448568));
#8110=CARTESIAN_POINT('Ctrl Pts',(-0.113804143538063,4.1170785121678,2.00063044772756));
#8111=CARTESIAN_POINT('Ctrl Pts',(-0.170251546647037,4.13961012941977,1.9966283083309));
#8112=CARTESIAN_POINT('Ctrl Pts',(-0.226538817597707,4.16227681169085,1.99022135678075));
#8113=CARTESIAN_POINT('Ctrl Pts',(-0.283517324840411,4.18522185233926,1.98373572460959));
#8114=CARTESIAN_POINT('Ctrl Pts',(-0.340330980874181,4.2083050095594,1.97478568883428));
#8115=CARTESIAN_POINT('Ctrl Pts',(-0.396662939840692,4.23139887703244,1.96340505169506));
#8116=CARTESIAN_POINT('Ctrl Pts',(-0.452300578028994,4.25420810054262,1.95216468684497));
#8117=CARTESIAN_POINT('Ctrl Pts',(-0.507467601032612,4.27702746883328,1.9385535132022));
#8118=CARTESIAN_POINT('Ctrl Pts',(-0.561868536406803,4.29973384084417,1.92265561988122));
#8119=CARTESIAN_POINT('Ctrl Pts',(-0.617287803103484,4.32286525352173,1.90646013383284));
#8120=CARTESIAN_POINT('Ctrl Pts',(-0.671911257239761,4.34587908012621,1.88789169564045));
#8121=CARTESIAN_POINT('Ctrl Pts',(-0.725448204174809,4.36864946353514,1.86709019276634));
#8122=CARTESIAN_POINT('Ctrl Pts',(-0.778985151109857,4.39141984694406,1.84628868989224));
#8123=CARTESIAN_POINT('Ctrl Pts',(-0.831434982711863,4.41394650592118,1.82325463286298));
#8124=CARTESIAN_POINT('Ctrl Pts',(-0.882538907291288,4.43611242205175,1.79817295107612));
#8125=CARTESIAN_POINT('Ctrl Pts',(-0.889702436356276,4.43921954514964,1.79465710844842));
#8126=CARTESIAN_POINT('Ctrl Pts',(-0.896839578793813,4.44231959797394,1.79110109618599));
#8127=CARTESIAN_POINT('Ctrl Pts',(-0.903949681684058,4.44541227674011,1.78750548470431));
#8128=CARTESIAN_POINT('Ctrl Pts',(-0.95381758158599,4.46710329830775,1.76228706012975));
#8129=CARTESIAN_POINT('Ctrl Pts',(-1.00290422621005,4.48915796079764,1.7348386881274));
#8130=CARTESIAN_POINT('Ctrl Pts',(-1.05092079729589,4.51146663811263,1.70524671607237));
#8131=CARTESIAN_POINT('Ctrl Pts',(-1.09887250320882,4.5337451788273,1.67569471955788));
#8132=CARTESIAN_POINT('Ctrl Pts',(-1.14575631859328,4.55627679608531,1.64400506360812));
#8133=CARTESIAN_POINT('Ctrl Pts',(-1.1912990493832,4.57894347836249,1.61031284532021));
#8134=CARTESIAN_POINT('Ctrl Pts',(-1.23740106803856,4.60188851901054,1.57620686947931));
#8135=CARTESIAN_POINT('Ctrl Pts',(-1.28212811955707,4.6249716762303,1.54004908311658));
#8136=CARTESIAN_POINT('Ctrl Pts',(-1.32522270849651,4.64806554370296,1.50202718275994));
#8137=CARTESIAN_POINT('Ctrl Pts',(-1.36778613414585,4.67087476721149,1.46447392216032));
#8138=CARTESIAN_POINT('Ctrl Pts',(-1.40875659069372,4.69369413550049,1.42510278851133));
#8139=CARTESIAN_POINT('Ctrl Pts',(-1.44792023605415,4.71640050750975,1.38413434134462));
#8140=CARTESIAN_POINT('Ctrl Pts',(-1.48781698584889,4.73953192018755,1.34239900565136));
#8141=CARTESIAN_POINT('Ctrl Pts',(-1.52583806567761,4.76254574679229,1.29900653939958));
#8142=CARTESIAN_POINT('Ctrl Pts',(-1.56180167032779,4.78531613020146,1.25422343600572));
#8143=CARTESIAN_POINT('Ctrl Pts',(-1.59776527497796,4.80808651361063,1.20944033261186));
#8144=CARTESIAN_POINT('Ctrl Pts',(-1.63167113305526,4.830613172588,1.16326733827078));
#8145=CARTESIAN_POINT('Ctrl Pts',(-1.66338758908104,4.85277908871881,1.11599400238347));
#8146=CARTESIAN_POINT('Ctrl Pts',(-1.66783346591803,4.85588621181656,1.10936742881996));
#8147=CARTESIAN_POINT('Ctrl Pts',(-1.67223640644797,4.85898626464074,1.10271926064603));
#8148=CARTESIAN_POINT('Ctrl Pts',(-1.67659613043342,4.86207894340678,1.09605031831591));
#8149=CARTESIAN_POINT('Ctrl Pts',(-1.7071737862946,4.88376996497442,1.04927657203996));
#8150=CARTESIAN_POINT('Ctrl Pts',(-1.73595988152442,4.90582462746431,1.00096226228135));
#8151=CARTESIAN_POINT('Ctrl Pts',(-1.76274746585988,4.92813330477931,0.951326577190672));
#8152=CARTESIAN_POINT('Ctrl Pts',(-1.78949886307729,4.95041184549336,0.901757944521465));
#8153=CARTESIAN_POINT('Ctrl Pts',(-1.81425661025109,4.97294346275075,0.85087198974096));
#8154=CARTESIAN_POINT('Ctrl Pts',(-1.83685166292844,4.99561014502732,0.798922307400261));
#8155=CARTESIAN_POINT('Ctrl Pts',(-1.8597241943295,5.01855518567546,0.746334656573327));
#8156=CARTESIAN_POINT('Ctrl Pts',(-1.88038006399974,5.04163834289532,0.692657569279139));
#8157=CARTESIAN_POINT('Ctrl Pts',(-1.89869012260881,5.06473221036808,0.638182343200189));
#8158=CARTESIAN_POINT('Ctrl Pts',(-1.91677450019352,5.08754143387663,0.584378552701312));
#8159=CARTESIAN_POINT('Ctrl Pts',(-1.93257038954424,5.11036080216563,0.529796922511562));
#8160=CARTESIAN_POINT('Ctrl Pts',(-1.94600287774792,5.1330671741749,0.47473538383138));
#8161=CARTESIAN_POINT('Ctrl Pts',(-1.95968680875216,5.15619858685286,0.418643147987838));
#8162=CARTESIAN_POINT('Ctrl Pts',(-1.97091779663741,5.17921241345773,0.362053629966241));
#8163=CARTESIAN_POINT('Ctrl Pts',(-1.97967164017932,5.20198279686705,0.305288522441415));
#8164=CARTESIAN_POINT('Ctrl Pts',(-1.98842548372123,5.22475318027637,0.24852341491659));
#8165=CARTESIAN_POINT('Ctrl Pts',(-1.99470232098284,5.24727983925388,0.191583499809409));
#8166=CARTESIAN_POINT('Ctrl Pts',(-1.99853290967558,5.26944575538484,0.134785361996117));
#8167=CARTESIAN_POINT('Ctrl Pts',(-1.9990698651768,5.27255287848279,0.12682364253107));
#8168=CARTESIAN_POINT('Ctrl Pts',(-1.99955883944015,5.27565293130716,0.11886468973834));
#8169=CARTESIAN_POINT('Ctrl Pts',(-2.,5.2787456100734,0.110909354270861));
#8170=CARTESIAN_POINT('Ctrl Pts',(-2.0030941536262,5.30043663164251,0.0551132738313546));
#8171=CARTESIAN_POINT('Ctrl Pts',(-2.00386648849157,5.32249129413392,-0.00112119340466367));
#8172=CARTESIAN_POINT('Ctrl Pts',(-2.00224737448632,5.34479997145046,-0.0575007497989892));
#8173=CARTESIAN_POINT('Ctrl Pts',(-2.00063044772871,5.36707851216043,-0.113804143519675));
#8174=CARTESIAN_POINT('Ctrl Pts',(-1.99662830833229,5.38961012941363,-0.170251546631835));
#8175=CARTESIAN_POINT('Ctrl Pts',(-1.99022135678213,5.41227681168596,-0.22653881758568));
#8176=CARTESIAN_POINT('Ctrl Pts',(-1.98373572461123,5.43522185233474,-0.283517324829355));
#8177=CARTESIAN_POINT('Ctrl Pts',(-1.97478568883606,5.45830500955525,-0.340330980864099));
#8178=CARTESIAN_POINT('Ctrl Pts',(-1.96340505169692,5.48139887702867,-0.39666293983159));
#8179=CARTESIAN_POINT('Ctrl Pts',(-1.95216468684977,5.50420810053341,-0.452300578006675));
#8180=CARTESIAN_POINT('Ctrl Pts',(-1.93855351321107,5.52702746881863,-0.507467600997336));
#8181=CARTESIAN_POINT('Ctrl Pts',(-1.92265561989521,5.54973384082418,-0.561868536359007));
#8182=CARTESIAN_POINT('Ctrl Pts',(-1.90646013384591,5.57286525350508,-0.617287803063998));
#8183=CARTESIAN_POINT('Ctrl Pts',(-1.88789169565188,5.59587908011291,-0.671911257208426));
#8184=CARTESIAN_POINT('Ctrl Pts',(-1.86709019277549,5.61864946352513,-0.725448204151379));
#8185=CARTESIAN_POINT('Ctrl Pts',(-1.84628868989909,5.64141984693736,-0.778985151094332));
#8186=CARTESIAN_POINT('Ctrl Pts',(-1.82325463286685,5.66394650591773,-0.831434982704001));
#8187=CARTESIAN_POINT('Ctrl Pts',(-1.79817295107646,5.68611242205145,-0.882538907290695));
#8188=CARTESIAN_POINT('Ctrl Pts',(-1.79465710844866,5.68921954514943,-0.889702436355896));
#8189=CARTESIAN_POINT('Ctrl Pts',(-1.79110109618612,5.69231959797383,-0.896839578793643));
#8190=CARTESIAN_POINT('Ctrl Pts',(-1.78750548470433,5.69541227674009,-0.903949681684095));
#8191=CARTESIAN_POINT('Ctrl Pts',(-1.76228706012609,5.7171032983109,-0.953817581593325));
#8192=CARTESIAN_POINT('Ctrl Pts',(-1.73483868811939,5.73915796080408,-1.00290422622447));
#8193=CARTESIAN_POINT('Ctrl Pts',(-1.70524671605941,5.7614666381224,-1.05092079731701));
#8194=CARTESIAN_POINT('Ctrl Pts',(-1.67569471954416,5.78374517883724,-1.09887250322985));
#8195=CARTESIAN_POINT('Ctrl Pts',(-1.64400506359364,5.80627679609541,-1.14575631861415));
#8196=CARTESIAN_POINT('Ctrl Pts',(-1.61031284530496,5.82894347837275,-1.19129904940391));
#8197=CARTESIAN_POINT('Ctrl Pts',(-1.57620686946479,5.85188851901994,-1.23740106805705));
#8198=CARTESIAN_POINT('Ctrl Pts',(-1.54004908310295,5.87497167623883,-1.28212811957342));
#8199=CARTESIAN_POINT('Ctrl Pts',(-1.50202718274738,5.89806554371058,-1.32522270851082));
#8200=CARTESIAN_POINT('Ctrl Pts',(-1.46447392215038,5.92087476721728,-1.36778613415636));
#8201=CARTESIAN_POINT('Ctrl Pts',(-1.42510278850434,5.94369413550442,-1.40875659070067));
#8202=CARTESIAN_POINT('Ctrl Pts',(-1.38413434134083,5.96640050751184,-1.44792023605782));
#8203=CARTESIAN_POINT('Ctrl Pts',(-1.34239900564825,5.98953192018921,-1.4878169858517));
#8204=CARTESIAN_POINT('Ctrl Pts',(-1.29900653939721,6.01254574679351,-1.52583806567962));
#8205=CARTESIAN_POINT('Ctrl Pts',(-1.25422343600415,6.03531613020225,-1.56180167032907));
#8206=CARTESIAN_POINT('Ctrl Pts',(-1.2094403326111,6.05808651361099,-1.59776527497852));
#8207=CARTESIAN_POINT('Ctrl Pts',(-1.1632673382709,6.08061317258793,-1.63167113305516));
#8208=CARTESIAN_POINT('Ctrl Pts',(-1.11599400238451,6.10277908871833,-1.66338758908036));
#8209=CARTESIAN_POINT('Ctrl Pts',(-1.10936742882066,6.10588621181624,-1.66783346591758));
#8210=CARTESIAN_POINT('Ctrl Pts',(-1.1027192606464,6.10898626464057,-1.67223640644774));
#8211=CARTESIAN_POINT('Ctrl Pts',(-1.09605031831594,6.11207894340677,-1.67659613043341));
#8212=CARTESIAN_POINT('Ctrl Pts',(-1.04927657203408,6.13376996497715,-1.70717378629846));
#8213=CARTESIAN_POINT('Ctrl Pts',(-1.00096226226917,6.15582462746988,-1.73595988153168));
#8214=CARTESIAN_POINT('Ctrl Pts',(-0.951326577171912,6.17813330478775,-1.76274746587001));
#8215=CARTESIAN_POINT('Ctrl Pts',(-0.901757944513397,6.20041184549692,-1.78949886308099));
#8216=CARTESIAN_POINT('Ctrl Pts',(-0.85087198974423,6.22294346274929,-1.81425661024918));
#8217=CARTESIAN_POINT('Ctrl Pts',(-0.798922307415297,6.24561014502079,-1.83685166292192));
#8218=CARTESIAN_POINT('Ctrl Pts',(-0.746334656587136,6.26855518566954,-1.85972419432402));
#8219=CARTESIAN_POINT('Ctrl Pts',(-0.692657569291611,6.29163834289003,-1.88038006399521));
#8220=CARTESIAN_POINT('Ctrl Pts',(-0.638182343211294,6.31473221036342,-1.8986901226051));
#8221=CARTESIAN_POINT('Ctrl Pts',(-0.584378552714839,6.33754143387098,-1.91677450018935));
#8222=CARTESIAN_POINT('Ctrl Pts',(-0.529796922527578,6.36036080215901,-1.93257038953981));
#8223=CARTESIAN_POINT('Ctrl Pts',(-0.474735383849875,6.38306717416733,-1.94600287774344));
#8224=CARTESIAN_POINT('Ctrl Pts',(-0.418643148002995,6.40619858684674,-1.95968680874906));
#8225=CARTESIAN_POINT('Ctrl Pts',(-0.362053629977934,6.42921241345308,-1.9709177966354));
#8226=CARTESIAN_POINT('Ctrl Pts',(-0.305288522449613,6.45198279686383,-1.97967164017809));
#8227=CARTESIAN_POINT('Ctrl Pts',(-0.248523414921292,6.47475318027459,-1.98842548372078));
#8228=CARTESIAN_POINT('Ctrl Pts',(-0.191583499810573,6.49727983925352,-1.99470232098286));
#8229=CARTESIAN_POINT('Ctrl Pts',(-0.134785361993779,6.51944575538583,-1.99853290967577));
#8230=CARTESIAN_POINT('Ctrl Pts',(-0.126823642529531,6.52255287848348,-1.99906986517692));
#8231=CARTESIAN_POINT('Ctrl Pts',(-0.118864689737606,6.52565293130753,-1.99955883944021));
#8232=CARTESIAN_POINT('Ctrl Pts',(-0.110909354270919,6.52874561007346,-2.00000000000002));
#8233=CARTESIAN_POINT('Ctrl Pts',(-0.0551132738396572,6.55043663163936,
-2.00309415362574));
#8234=CARTESIAN_POINT('Ctrl Pts',(0.00112119338795719,6.57249129412745,
-2.00386648849135));
#8235=CARTESIAN_POINT('Ctrl Pts',(0.0575007497738815,6.5947999714406,-2.00224737448704));
#8236=CARTESIAN_POINT('Ctrl Pts',(0.113804143520435,6.61707851216074,-2.00063044772938));
#8237=CARTESIAN_POINT('Ctrl Pts',(0.170251546658587,6.63961012942435,-1.99662830833074));
#8238=CARTESIAN_POINT('Ctrl Pts',(0.226538817638237,6.6622768117072,-1.99022135677613));
#8239=CARTESIAN_POINT('Ctrl Pts',(0.283517324877466,6.6852218523543,-1.9837357246042));
#8240=CARTESIAN_POINT('Ctrl Pts',(0.340330980907712,6.70830500957309,-1.9747856888284));
#8241=CARTESIAN_POINT('Ctrl Pts',(0.396662939870692,6.73139887704476,-1.96340505168901));
#8242=CARTESIAN_POINT('Ctrl Pts',(0.452300578056111,6.75420810055383,-1.95216468683862));
#8243=CARTESIAN_POINT('Ctrl Pts',(0.507467601056806,6.77702746884334,-1.93855351319579));
#8244=CARTESIAN_POINT('Ctrl Pts',(0.561868536428129,6.79973384085308,-1.92265561987499));
#8245=CARTESIAN_POINT('Ctrl Pts',(0.617287803120988,6.8228652535291,-1.90646013382708));
#8246=CARTESIAN_POINT('Ctrl Pts',(0.671911257253534,6.84587908013206,-1.88789169563546));
#8247=CARTESIAN_POINT('Ctrl Pts',(0.725448204184969,6.86864946353947,-1.86709019276243));
#8248=CARTESIAN_POINT('Ctrl Pts',(0.778985151116403,6.89141984694689,-1.84628868988941));
#8249=CARTESIAN_POINT('Ctrl Pts',(0.831434982714933,6.91394650592253,-1.8232546328615));
#8250=CARTESIAN_POINT('Ctrl Pts',(0.882538907291036,6.93611242205166,-1.79817295107629));
#8251=CARTESIAN_POINT('Ctrl Pts',(0.889702436356114,6.93921954514958,-1.79465710844855));
#8252=CARTESIAN_POINT('Ctrl Pts',(0.896839578793735,6.94231959797392,-1.79110109618609));
#8253=CARTESIAN_POINT('Ctrl Pts',(0.903949681684065,6.94541227674013,-1.78750548470436));
#8254=CARTESIAN_POINT('Ctrl Pts',(0.953817581589804,6.96710329830942,-1.7622870601279));
#8255=CARTESIAN_POINT('Ctrl Pts',(1.00290422621755,6.98915796080102,-1.7348386881233));
#8256=CARTESIAN_POINT('Ctrl Pts',(1.0509207973069,7.01146663811774,-1.70524671606568));
#8257=CARTESIAN_POINT('Ctrl Pts',(1.09887250321008,7.03374517882799,-1.67569471955678));
#8258=CARTESIAN_POINT('Ctrl Pts',(1.14575631858522,7.05627679608148,-1.64400506361347));
#8259=CARTESIAN_POINT('Ctrl Pts',(1.19129904936639,7.07894347835411,-1.61031284533278));
#8260=CARTESIAN_POINT('Ctrl Pts',(1.23740106802345,7.1018885190028,-1.57620686949137));
#8261=CARTESIAN_POINT('Ctrl Pts',(1.2821281195436,7.12497167622323,-1.54004908312799));
#8262=CARTESIAN_POINT('Ctrl Pts',(1.32522270848461,7.14806554369656,-1.50202718277058));
#8263=CARTESIAN_POINT('Ctrl Pts',(1.36778613412793,7.1708747672017,-1.46447392217686));
#8264=CARTESIAN_POINT('Ctrl Pts',(1.40875659067027,7.19369413548732,-1.42510278853431));
#8265=CARTESIAN_POINT('Ctrl Pts',(1.44792023602575,7.21640050749326,-1.38413434137446));
#8266=CARTESIAN_POINT('Ctrl Pts',(1.48781698582602,7.23953192017381,-1.34239900567713));
#8267=CARTESIAN_POINT('Ctrl Pts',(1.52583806565988,7.26254574678129,-1.29900653942082));
#8268=CARTESIAN_POINT('Ctrl Pts',(1.56180167031475,7.28531613019319,-1.25422343602206));
#8269=CARTESIAN_POINT('Ctrl Pts',(1.59776527496962,7.30808651360508,-1.2094403326233));
#8270=CARTESIAN_POINT('Ctrl Pts',(1.63167113305116,7.33061317258512,-1.16326733827696));
#8271=CARTESIAN_POINT('Ctrl Pts',(1.66338758908065,7.35277908871853,-1.11599400238413));
#8272=CARTESIAN_POINT('Ctrl Pts',(1.66783346591777,7.35588621181638,-1.10936742882042));
#8273=CARTESIAN_POINT('Ctrl Pts',(1.67223640644784,7.35898626464064,-1.10271926064629));
#8274=CARTESIAN_POINT('Ctrl Pts',(1.67659613043342,7.36207894340678,-1.09605031831597));
#8275=CARTESIAN_POINT('Ctrl Pts',(1.70717378629979,7.3837699649781,-1.04927657203209));
#8276=CARTESIAN_POINT('Ctrl Pts',(1.73595988153417,7.40582462747179,-1.00096226226504));
#8277=CARTESIAN_POINT('Ctrl Pts',(1.76274746587349,7.42813330479065,-0.951326577165512));
#8278=CARTESIAN_POINT('Ctrl Pts',(1.78949886308338,7.45041184549909,-0.901757944508564));
#8279=CARTESIAN_POINT('Ctrl Pts',(1.81425661025064,7.47294346275071,-0.85087198974103));
#8280=CARTESIAN_POINT('Ctrl Pts',(1.83685166292257,7.49561014502146,-0.798922307413823));
#8281=CARTESIAN_POINT('Ctrl Pts',(1.85972419432456,7.51855518567013,-0.746334656585818));
#8282=CARTESIAN_POINT('Ctrl Pts',(1.88038006399563,7.54163834289054,-0.692657569290468));
#8283=CARTESIAN_POINT('Ctrl Pts',(1.89869012260542,7.56473221036385,-0.638182343210334));
#8284=CARTESIAN_POINT('Ctrl Pts',(1.91677450018888,7.58754143387044,-0.584378552716151));
#8285=CARTESIAN_POINT('Ctrl Pts',(1.93257038953873,7.6103608021575,-0.529796922531237));
#8286=CARTESIAN_POINT('Ctrl Pts',(1.94600287774196,7.63306717416486,-0.474735383855908));
#8287=CARTESIAN_POINT('Ctrl Pts',(1.95968680874796,7.65619858684464,-0.418643148008195));
#8288=CARTESIAN_POINT('Ctrl Pts',(1.97091779663461,7.67921241345134,-0.362053629982299));
#8289=CARTESIAN_POINT('Ctrl Pts',(1.97967164017753,7.70198279686246,-0.305288522453109));
#8290=CARTESIAN_POINT('Ctrl Pts',(1.98842548372046,7.72475318027358,-0.248523414923918));
#8291=CARTESIAN_POINT('Ctrl Pts',(1.99470232098269,7.74727983925285,-0.191583499812325));
#8292=CARTESIAN_POINT('Ctrl Pts',(1.99853290967569,7.76944575538552,-0.134785361994661));
#8293=CARTESIAN_POINT('Ctrl Pts',(1.99906986517686,7.77255287848327,-0.126823642530115));
#8294=CARTESIAN_POINT('Ctrl Pts',(1.99955883944017,7.77565293130744,-0.11886468973791));
#8295=CARTESIAN_POINT('Ctrl Pts',(2.,7.77874561007349,-0.110909354270931));
#8296=CARTESIAN_POINT('Ctrl Pts',(2.00309415362605,7.80043663164154,-0.0551132738341087));
#8297=CARTESIAN_POINT('Ctrl Pts',(2.00386648849149,7.82249129413187,0.00112119339916694));
#8298=CARTESIAN_POINT('Ctrl Pts',(2.00224737448655,7.84479997144731,0.057500749790785));
#8299=CARTESIAN_POINT('Ctrl Pts',(2.00063044772897,7.8670785121599,0.113804143518177));
#8300=CARTESIAN_POINT('Ctrl Pts',(1.99662830833203,7.88961012941579,0.170251546637083));
#8301=CARTESIAN_POINT('Ctrl Pts',(1.99022135678076,7.91227681169085,0.22653881759762));
#8302=CARTESIAN_POINT('Ctrl Pts',(1.98373572460961,7.93522185233927,0.283517324840359));
#8303=CARTESIAN_POINT('Ctrl Pts',(1.97478568883429,7.95830500955941,0.340330980874146));
#8304=CARTESIAN_POINT('Ctrl Pts',(1.96340505169508,7.98139887703245,0.396662939840668));
#8305=CARTESIAN_POINT('Ctrl Pts',(1.95216468684763,8.00420810053727,0.452300578015884));
#8306=CARTESIAN_POINT('Ctrl Pts',(1.93855351320864,8.02702746882255,0.507467601006632));
#8307=CARTESIAN_POINT('Ctrl Pts',(1.92265561989246,8.04973384082815,0.561868536368393));
#8308=CARTESIAN_POINT('Ctrl Pts',(1.90646013384331,8.07286525350844,0.617287803071861));
#8309=CARTESIAN_POINT('Ctrl Pts',(1.88789169564955,8.09587908011566,0.6719112572148));
#8310=CARTESIAN_POINT('Ctrl Pts',(1.86709019277355,8.11864946352728,0.725448204156317));
#8311=CARTESIAN_POINT('Ctrl Pts',(1.84628868989755,8.14141984693891,0.778985151097833));
#8312=CARTESIAN_POINT('Ctrl Pts',(1.82325463286583,8.16394650591869,0.831434982706109));
#8313=CARTESIAN_POINT('Ctrl Pts',(1.79817295107606,8.18611242205183,0.882538907291475));
#8314=CARTESIAN_POINT('Ctrl Pts',(1.79465710844839,8.1892195451497,0.889702436356406));
#8315=CARTESIAN_POINT('Ctrl Pts',(1.79110109618599,8.19231959797397,0.896839578793874));
#8316=CARTESIAN_POINT('Ctrl Pts',(1.78750548470434,8.19541227674012,0.903949681684059));
#8317=CARTESIAN_POINT('Ctrl Pts',(1.7622870601238,8.21710329831291,0.953817581597852));
#8318=CARTESIAN_POINT('Ctrl Pts',(1.73483868811439,8.23915796080813,1.0029042262334));
#8319=CARTESIAN_POINT('Ctrl Pts',(1.70524671605131,8.26146663812854,1.05092079733016));
#8320=CARTESIAN_POINT('Ctrl Pts',(1.67569471954768,8.28374517883438,1.09887250322331));
#8321=CARTESIAN_POINT('Ctrl Pts',(1.64400506361051,8.30627679608333,1.14575631858882));
#8322=CARTESIAN_POINT('Ctrl Pts',(1.61031284533679,8.32894347835137,1.19129904936089));
#8323=CARTESIAN_POINT('Ctrl Pts',(1.57620686949512,8.35188851900034,1.23740106801864));
#8324=CARTESIAN_POINT('Ctrl Pts',(1.5400490831314,8.37497167622106,1.28212811953947));
#8325=CARTESIAN_POINT('Ctrl Pts',(1.50202718277361,8.39806554369468,1.3252227084811));
#8326=CARTESIAN_POINT('Ctrl Pts',(1.46447392217283,8.42087476720419,1.36778613413263));
#8327=CARTESIAN_POINT('Ctrl Pts',(1.42510278852252,8.44369413549416,1.40875659068257));
#8328=CARTESIAN_POINT('Ctrl Pts',(1.38413434135432,8.4664005075044,1.44792023604494));
#8329=CARTESIAN_POINT('Ctrl Pts',(1.34239900565957,8.48953192018319,1.48781698584163));
#8330=CARTESIAN_POINT('Ctrl Pts',(1.29900653940613,8.51254574678892,1.52583806567217));
#8331=CARTESIAN_POINT('Ctrl Pts',(1.25422343601048,8.53531613019907,1.561801670324));
#8332=CARTESIAN_POINT('Ctrl Pts',(1.20944033261483,8.55808651360922,1.59776527497583));
#8333=CARTESIAN_POINT('Ctrl Pts',(1.16326733827184,8.58061317258754,1.63167113305461));
#8334=CARTESIAN_POINT('Ctrl Pts',(1.11599400238253,8.60277908871928,1.66338758908168));
#8335=CARTESIAN_POINT('Ctrl Pts',(1.10936742881934,8.60588621181689,1.66783346591845));
#8336=CARTESIAN_POINT('Ctrl Pts',(1.10271926064574,8.60898626464091,1.67223640644817));
#8337=CARTESIAN_POINT('Ctrl Pts',(1.09605031831595,8.6120789434068,1.6765961304334));
#8338=CARTESIAN_POINT('Ctrl Pts',(1.0492765720318,8.63376996497824,1.70717378629997));
#8339=CARTESIAN_POINT('Ctrl Pts',(1.00096226226444,8.65582462747207,1.73595988153451));
#8340=CARTESIAN_POINT('Ctrl Pts',(0.951326577164588,8.67813330479107,1.76274746587397));
#8341=CARTESIAN_POINT('Ctrl Pts',(0.90175794451587,8.70041184549581,1.78949886307939));
#8342=CARTESIAN_POINT('Ctrl Pts',(0.850871989756991,8.72294346274365,1.81425661024285));
#8343=CARTESIAN_POINT('Ctrl Pts',(0.798922307438777,8.74561014501057,1.83685166291171));
#8344=CARTESIAN_POINT('Ctrl Pts',(0.746334656609139,8.76855518566006,1.85972419431526));
#8345=CARTESIAN_POINT('Ctrl Pts',(0.692657569312053,8.79163834288131,1.88038006398774));
#8346=CARTESIAN_POINT('Ctrl Pts',(0.638182343230064,8.81473221035548,1.89869012259878));
#8347=CARTESIAN_POINT('Ctrl Pts',(0.58437855273512,8.83754143386247,1.91677450018311));
#8348=CARTESIAN_POINT('Ctrl Pts',(0.529796922549362,8.86036080214996,1.93257038953378));
#8349=CARTESIAN_POINT('Ctrl Pts',(0.474735383873144,8.88306717415774,1.94600287773775));
#8350=CARTESIAN_POINT('Ctrl Pts',(0.418643148022863,8.90619858683864,1.9596868087449));
#8351=CARTESIAN_POINT('Ctrl Pts',(0.362053629994299,8.92921241344647,1.97091779663247));
#8352=CARTESIAN_POINT('Ctrl Pts',(0.305288522462434,8.95198279685869,1.97967164017607));
#8353=CARTESIAN_POINT('Ctrl Pts',(0.24852341493057,8.97475318027092,1.98842548371968));
#8354=CARTESIAN_POINT('Ctrl Pts',(0.191583499816279,8.99727983925128,1.99470232098237));
#8355=CARTESIAN_POINT('Ctrl Pts',(0.13478536199593,9.01944575538499,1.99853290967558));
#8356=CARTESIAN_POINT('Ctrl Pts',(0.126823642530953,9.02255287848291,1.99906986517679));
#8357=CARTESIAN_POINT('Ctrl Pts',(0.118864689738311,9.02565293130725,1.99955883944013));
#8358=CARTESIAN_POINT('Ctrl Pts',(0.110909354270898,9.02874561007346,1.99999999999998));
#8359=CARTESIAN_POINT('Ctrl Pts',(0.0551132738224583,9.05043663164604,2.00309415362669));
#8360=CARTESIAN_POINT('Ctrl Pts',(-0.00112119342262139,9.07249129414105,
2.00386648849181));
#8361=CARTESIAN_POINT('Ctrl Pts',(-0.0575007498260162,9.09479997146124,
2.00224737448554));
#8362=CARTESIAN_POINT('Ctrl Pts',(-0.113804143546013,9.11707851217099,2.00063044772719));
#8363=CARTESIAN_POINT('Ctrl Pts',(-0.170251546657395,9.13961012942394,1.9966283083301));
#8364=CARTESIAN_POINT('Ctrl Pts',(-0.226538817610427,9.16227681169601,1.99022135677932));
#8365=CARTESIAN_POINT('Ctrl Pts',(-0.283517324852289,9.18522185234411,1.9837357246079));
#8366=CARTESIAN_POINT('Ctrl Pts',(-0.340330980885206,9.20830500956393,1.97478568883238));
#8367=CARTESIAN_POINT('Ctrl Pts',(-0.396662939850842,9.23139887703663,1.96340505169303));
#8368=CARTESIAN_POINT('Ctrl Pts',(-0.45230057804149,9.2542081005478,1.95216468684217));
#8369=CARTESIAN_POINT('Ctrl Pts',(-0.507467601047385,9.27702746883943,1.93855351319842));
#8370=CARTESIAN_POINT('Ctrl Pts',(-0.561868536423777,9.29973384085128,1.92265561987627));
#8371=CARTESIAN_POINT('Ctrl Pts',(-0.617287803117933,9.32286525352782,1.9064601338281));
#8372=CARTESIAN_POINT('Ctrl Pts',(-0.671911257251733,9.34587908013129,1.88789169563612));
#8373=CARTESIAN_POINT('Ctrl Pts',(-0.725448204184394,9.36864946353922,1.86709019276262));
#8374=CARTESIAN_POINT('Ctrl Pts',(-0.778985151117054,9.39141984694716,1.84628868988913));
#8375=CARTESIAN_POINT('Ctrl Pts',(-0.831434982716753,9.41394650592329,1.82325463286067));
#8376=CARTESIAN_POINT('Ctrl Pts',(-0.882538907293985,9.43611242205291,1.7981729510748));
#8377=CARTESIAN_POINT('Ctrl Pts',(-0.889702436358074,9.43921954515041,1.79465710844753));
#8378=CARTESIAN_POINT('Ctrl Pts',(-0.896839578794715,9.44231959797432,1.79110109618554));
#8379=CARTESIAN_POINT('Ctrl Pts',(-0.903949681684071,9.44541227674011,1.7875054847043));
#8380=CARTESIAN_POINT('Ctrl Pts',(-0.95381758159861,9.46710329831322,1.7622870601234));
#8381=CARTESIAN_POINT('Ctrl Pts',(-1.00290422623487,9.48915796080878,1.73483868811356));
#8382=CARTESIAN_POINT('Ctrl Pts',(-1.05092079733231,9.51146663812953,1.70524671604998));
#8383=CARTESIAN_POINT('Ctrl Pts',(-1.09887250322587,9.53374517883558,1.67569471954602));
#8384=CARTESIAN_POINT('Ctrl Pts',(-1.14575631859174,9.55627679608474,1.6440050636085));
#8385=CARTESIAN_POINT('Ctrl Pts',(-1.19129904936418,9.578943478353,1.61031284533437));
#8386=CARTESIAN_POINT('Ctrl Pts',(-1.23740106802143,9.60188851900177,1.57620686949291));
#8387=CARTESIAN_POINT('Ctrl Pts',(-1.28212811954179,9.62497167622228,1.54004908312946));
#8388=CARTESIAN_POINT('Ctrl Pts',(-1.32522270848299,9.64806554369569,1.50202718277195));
#8389=CARTESIAN_POINT('Ctrl Pts',(-1.36778613412685,9.67087476720111,1.46447392217784));
#8390=CARTESIAN_POINT('Ctrl Pts',(-1.4087565906697,9.693694135487,1.42510278853486));
#8391=CARTESIAN_POINT('Ctrl Pts',(-1.44792023602563,9.7164005074932,1.38413434137453));
#8392=CARTESIAN_POINT('Ctrl Pts',(-1.48781698582588,9.73953192017373,1.34239900567723));
#8393=CARTESIAN_POINT('Ctrl Pts',(-1.52583806565969,9.76254574678119,1.29900653942098));
#8394=CARTESIAN_POINT('Ctrl Pts',(-1.56180167031453,9.78531613019306,1.25422343602228));
#8395=CARTESIAN_POINT('Ctrl Pts',(-1.59776527496938,9.80808651360493,1.20944033262357));
#8396=CARTESIAN_POINT('Ctrl Pts',(-1.63167113305088,9.83061317258494,1.16326733827729));
#8397=CARTESIAN_POINT('Ctrl Pts',(-1.66338758908036,9.85277908871833,1.11599400238452));
#8398=CARTESIAN_POINT('Ctrl Pts',(-1.66783346591758,9.85588621181624,1.10936742882067));
#8399=CARTESIAN_POINT('Ctrl Pts',(-1.67223640644775,9.85898626464057,1.1027192606464));
#8400=CARTESIAN_POINT('Ctrl Pts',(-1.67659613043342,9.86207894340678,1.09605031831594));
#8401=CARTESIAN_POINT('Ctrl Pts',(-1.70717378629812,9.88376996497691,1.04927657203461));
#8402=CARTESIAN_POINT('Ctrl Pts',(-1.73595988153104,9.90582462746939,1.00096226227027));
#8403=CARTESIAN_POINT('Ctrl Pts',(-1.7627474658691,9.928133304787,0.951326577173604));
#8404=CARTESIAN_POINT('Ctrl Pts',(-1.78949886308675,9.95041184550169,0.90175794450282));
#8405=CARTESIAN_POINT('Ctrl Pts',(-1.81425661026064,9.97294346275971,0.850871989720727));
#8406=CARTESIAN_POINT('Ctrl Pts',(-1.83685166293795,9.99561014503689,0.798922307378422));
#8407=CARTESIAN_POINT('Ctrl Pts',(-1.85972419433764,10.0185551856843,0.746334656552911));
#8408=CARTESIAN_POINT('Ctrl Pts',(-1.88038006400666,10.0416383429035,0.692657569260229));
#8409=CARTESIAN_POINT('Ctrl Pts',(-1.89869012261463,10.0647322103755,0.638182343182895));
#8410=CARTESIAN_POINT('Ctrl Pts',(-1.91677450019885,10.087541433884,0.584378552683838));
#8411=CARTESIAN_POINT('Ctrl Pts',(-1.93257038954908,10.110360802173,0.529796922493951));
#8412=CARTESIAN_POINT('Ctrl Pts',(-1.94600287775226,10.1330671741823,0.474735383813648));
#8413=CARTESIAN_POINT('Ctrl Pts',(-1.95968680875531,10.1561985868591,0.418643147972745));
#8414=CARTESIAN_POINT('Ctrl Pts',(-1.97091779663961,10.1792124134628,0.36205362995384));
#8415=CARTESIAN_POINT('Ctrl Pts',(-1.97967164018081,10.201982796871,0.305288522431753));
#8416=CARTESIAN_POINT('Ctrl Pts',(-1.98842548372202,10.2247531802792,0.248523414909664));
#8417=CARTESIAN_POINT('Ctrl Pts',(-1.99470232098315,10.2472798392556,0.191583499805278));
#8418=CARTESIAN_POINT('Ctrl Pts',(-1.99853290967567,10.2694457553855,0.13478536199476));
#8419=CARTESIAN_POINT('Ctrl Pts',(-1.99906986517685,10.2725528784832,0.126823642530179));
#8420=CARTESIAN_POINT('Ctrl Pts',(-1.99955883944017,10.2756529313074,0.118864689737915));
#8421=CARTESIAN_POINT('Ctrl Pts',(-2.,10.2787456100735,0.110909354270896));
#8422=CARTESIAN_POINT('Ctrl Pts',(-2.00309415362599,10.3004366316412,0.0551132738350213));
#8423=CARTESIAN_POINT('Ctrl Pts',(-2.00386648849147,10.3224912941311,-0.00112119339731515));
#8424=CARTESIAN_POINT('Ctrl Pts',(-2.00224737448664,10.3447999714462,-0.0575007497879437));
#8425=CARTESIAN_POINT('Ctrl Pts',(-2.00063044772864,10.3670785121657,-0.113804143532892));
#8426=CARTESIAN_POINT('Ctrl Pts',(-1.99662830832979,10.3896101294287,-0.170251546669399));
#8427=CARTESIAN_POINT('Ctrl Pts',(-1.99022135677511,10.4122768117109,-0.226538817647384));
#8428=CARTESIAN_POINT('Ctrl Pts',(-1.983735724603,10.4352218523577,-0.283517324885871));
#8429=CARTESIAN_POINT('Ctrl Pts',(-1.97478568882708,10.4583050095762,-0.340330980915366));
#8430=CARTESIAN_POINT('Ctrl Pts',(-1.96340505168762,10.4813988770476,-0.396662939877621));
#8431=CARTESIAN_POINT('Ctrl Pts',(-1.95216468683779,10.5042081005551,-0.452300578059234));
#8432=CARTESIAN_POINT('Ctrl Pts',(-1.93855351319585,10.5270274688431,-0.507467601056206));
#8433=CARTESIAN_POINT('Ctrl Pts',(-1.92265561987624,10.5497338408513,-0.561868536423899));
#8434=CARTESIAN_POINT('Ctrl Pts',(-1.90646013382819,10.5728652535277,-0.617287803117652));
#8435=CARTESIAN_POINT('Ctrl Pts',(-1.88789169563638,10.595879080131,-0.671911257251014));
#8436=CARTESIAN_POINT('Ctrl Pts',(-1.86709019276308,10.6186494635387,-0.725448204183275));
#8437=CARTESIAN_POINT('Ctrl Pts',(-1.84628868988979,10.6414198469465,-0.778985151115534));
#8438=CARTESIAN_POINT('Ctrl Pts',(-1.82325463286158,10.6639465059224,-0.831434982714827));
#8439=CARTESIAN_POINT('Ctrl Pts',(-1.79817295107597,10.6861124220519,-0.882538907291692));
#8440=CARTESIAN_POINT('Ctrl Pts',(-1.79465710844833,10.6892195451497,-0.889702436356563));
#8441=CARTESIAN_POINT('Ctrl Pts',(-1.79110109618594,10.692319597974,-0.896839578793999));
#8442=CARTESIAN_POINT('Ctrl Pts',(-1.78750548470432,10.6954122767401,-0.903949681684119));
#8443=CARTESIAN_POINT('Ctrl Pts',(-1.76228706013068,10.7171032983069,-0.953817581584232));
#8444=CARTESIAN_POINT('Ctrl Pts',(-1.7348386881294,10.739157960796,-1.00290422620656));
#8445=CARTESIAN_POINT('Ctrl Pts',(-1.70524671607559,10.7614666381102,-1.05092079729075));
#8446=CARTESIAN_POINT('Ctrl Pts',(-1.67569471957146,10.7837451788171,-1.09887250318719));
#8447=CARTESIAN_POINT('Ctrl Pts',(-1.64400506363352,10.8062767960673,-1.14575631855595));
#8448=CARTESIAN_POINT('Ctrl Pts',(-1.61031284535875,10.8289434783366,-1.19129904933118));
#8449=CARTESIAN_POINT('Ctrl Pts',(-1.57620686951628,10.8518885189866,-1.23740106799179));
#8450=CARTESIAN_POINT('Ctrl Pts',(-1.54004908315154,10.8749716762084,-1.28212811951541));
#8451=CARTESIAN_POINT('Ctrl Pts',(-1.50202718279246,10.8980655436832,-1.32522270845973));
#8452=CARTESIAN_POINT('Ctrl Pts',(-1.46447392219654,10.9208747671901,-1.36778613410698));
#8453=CARTESIAN_POINT('Ctrl Pts',(-1.4251027885515,10.9436941354775,-1.408756590653));
#8454=CARTESIAN_POINT('Ctrl Pts',(-1.38413434138884,10.9664005074852,-1.44792023601195));
#8455=CARTESIAN_POINT('Ctrl Pts',(-1.3423990056896,10.9895319201671,-1.48781698581485));
#8456=CARTESIAN_POINT('Ctrl Pts',(-1.29900653943119,11.0125457467759,-1.52583806565114));
#8457=CARTESIAN_POINT('Ctrl Pts',(-1.25422343603018,11.035316130189,-1.5618016703082));
#8458=CARTESIAN_POINT('Ctrl Pts',(-1.20944033262918,11.0580865136022,-1.59776527496527));
#8459=CARTESIAN_POINT('Ctrl Pts',(-1.1632673382804,11.0806131725835,-1.6316711330488));
#8460=CARTESIAN_POINT('Ctrl Pts',(-1.11599400238502,11.1027790887181,-1.66338758908006));
#8461=CARTESIAN_POINT('Ctrl Pts',(-1.10936742882101,11.1058862118161,-1.66783346591739));
#8462=CARTESIAN_POINT('Ctrl Pts',(-1.10271926064657,11.1089862646405,-1.67223640644766));
#8463=CARTESIAN_POINT('Ctrl Pts',(-1.09605031831595,11.1120789434068,-1.67659613043343));
#8464=CARTESIAN_POINT('Ctrl Pts',(-1.04927657204784,11.1337699649708,-1.70717378628948));
#8465=CARTESIAN_POINT('Ctrl Pts',(-1.00096226229761,11.1558246274569,-1.73595988151476));
#8466=CARTESIAN_POINT('Ctrl Pts',(-0.951326577215707,11.1781333047681,-1.76274746584638));
#8467=CARTESIAN_POINT('Ctrl Pts',(-0.901757944540899,11.2004118454848,-1.78949886306773));
#8468=CARTESIAN_POINT('Ctrl Pts',(-0.85087198975444,11.2229434627449,-1.814256610245));
#8469=CARTESIAN_POINT('Ctrl Pts',(-0.798922307407508,11.2456101450242,-1.8368516629253));
#8470=CARTESIAN_POINT('Ctrl Pts',(-0.746334656580119,11.2685551856726,-1.8597241943268));
#8471=CARTESIAN_POINT('Ctrl Pts',(-0.692657569285422,11.2916383428927,-1.88038006399746));
#8472=CARTESIAN_POINT('Ctrl Pts',(-0.638182343205964,11.3147322103657,-1.89869012260688));
#8473=CARTESIAN_POINT('Ctrl Pts',(-0.584378552711461,11.3375414338724,-1.91677450019031));
#8474=CARTESIAN_POINT('Ctrl Pts',(-0.529796922526239,11.3603608021596,-1.9325703895401));
#8475=CARTESIAN_POINT('Ctrl Pts',(-0.474735383850581,11.3830671741671,-1.94600287774326));
#8476=CARTESIAN_POINT('Ctrl Pts',(-0.418643148004073,11.4061985868463,-1.9596868087488));
#8477=CARTESIAN_POINT('Ctrl Pts',(-0.36205362997942,11.4292124134525,-1.97091779663511));
#8478=CARTESIAN_POINT('Ctrl Pts',(-0.30528852245147,11.4519827968631,-1.97967164017779));
#8479=CARTESIAN_POINT('Ctrl Pts',(-0.248523414923521,11.4747531802737,-1.98842548372048));
#8480=CARTESIAN_POINT('Ctrl Pts',(-0.191583499813202,11.4972798392525,-1.99470232098259));
#8481=CARTESIAN_POINT('Ctrl Pts',(-0.13478536199678,11.5194457553847,-1.99853290967556));
#8482=CARTESIAN_POINT('Ctrl Pts',(-0.126823642531537,11.5225528784827,-1.99906986517679));
#8483=CARTESIAN_POINT('Ctrl Pts',(-0.118864689738596,11.5256529313072,-1.99955883944015));
#8484=CARTESIAN_POINT('Ctrl Pts',(-0.110909354270918,11.5287456100735,-2.00000000000001));
#8485=CARTESIAN_POINT('Ctrl Pts',(-0.0551132738492376,11.5504366316357,
-2.00309415362522));
#8486=CARTESIAN_POINT('Ctrl Pts',(0.00112119336864007,11.5724912941199,
-2.0038664884911));
#8487=CARTESIAN_POINT('Ctrl Pts',(0.0575007497448667,11.5947999714292,-2.00224737448789));
#8488=CARTESIAN_POINT('Ctrl Pts',(0.113804143493782,11.6170785121502,-2.00063044773099));
#8489=CARTESIAN_POINT('Ctrl Pts',(0.170251546634363,11.6396101294147,-1.9966283083329));
#8490=CARTESIAN_POINT('Ctrl Pts',(0.226538817616414,11.6622768116985,-1.99022135677864));
#8491=CARTESIAN_POINT('Ctrl Pts',(0.283517324857556,11.6852218523463,-1.98373572460713));
#8492=CARTESIAN_POINT('Ctrl Pts',(0.340330980889751,11.7083050095658,-1.97478568883157));
#8493=CARTESIAN_POINT('Ctrl Pts',(0.396662939854681,11.7313988770382,-1.96340505169226));
#8494=CARTESIAN_POINT('Ctrl Pts',(0.452300578040246,11.7542081005473,-1.95216468684231));
#8495=CARTESIAN_POINT('Ctrl Pts',(0.507467601041112,11.7770274688369,-1.93855351319992));
#8496=CARTESIAN_POINT('Ctrl Pts',(0.561868536412669,11.7997338408467,-1.92265561987953));
#8497=CARTESIAN_POINT('Ctrl Pts',(0.617287803108415,11.8228652535238,-1.90646013383125));
#8498=CARTESIAN_POINT('Ctrl Pts',(0.671911257243793,11.8458790801279,-1.88789169563901));
#8499=CARTESIAN_POINT('Ctrl Pts',(0.725448204177951,11.8686494635365,-1.86709019276516));
#8500=CARTESIAN_POINT('Ctrl Pts',(0.778985151112109,11.891419846945,-1.8462886898913));
#8501=CARTESIAN_POINT('Ctrl Pts',(0.831434982713284,11.9139465059218,-1.82325463286234));
#8502=CARTESIAN_POINT('Ctrl Pts',(0.882538907291871,11.936112422052,-1.79817295107588));
#8503=CARTESIAN_POINT('Ctrl Pts',(0.889702436356676,11.9392195451498,-1.79465710844827));
#8504=CARTESIAN_POINT('Ctrl Pts',(0.896839578794011,11.942319597974,-1.79110109618594));
#8505=CARTESIAN_POINT('Ctrl Pts',(0.903949681684077,11.9454122767401,-1.78750548470435));
#8506=CARTESIAN_POINT('Ctrl Pts',(0.953817581596336,11.9671032983122,-1.7622870601246));
#8507=CARTESIAN_POINT('Ctrl Pts',(1.00290422623042,11.9891579608068,-1.73483868811609));
#8508=CARTESIAN_POINT('Ctrl Pts',(1.05092079732578,12.0114666381265,-1.70524671605404));
#8509=CARTESIAN_POINT('Ctrl Pts',(1.09887250322481,12.033745178835,-1.67569471954696));
#8510=CARTESIAN_POINT('Ctrl Pts',(1.14575631859591,12.0562767960867,-1.64400506360586));
#8511=CARTESIAN_POINT('Ctrl Pts',(1.19129904937325,12.0789434783575,-1.61031284532769));
#8512=CARTESIAN_POINT('Ctrl Pts',(1.23740106802966,12.101888519006,-1.57620686948646));
#8513=CARTESIAN_POINT('Ctrl Pts',(1.28212811954919,12.1249716762261,-1.5400490831233));
#8514=CARTESIAN_POINT('Ctrl Pts',(1.3252227084896,12.1480655436992,-1.50202718276616));
#8515=CARTESIAN_POINT('Ctrl Pts',(1.36778613413641,12.1708747672063,-1.46447392216911));
#8516=CARTESIAN_POINT('Ctrl Pts',(1.40875659068193,12.1936941354938,-1.42510278852297));
#8517=CARTESIAN_POINT('Ctrl Pts',(1.44792023604029,12.2164005075017,-1.38413434135923));
#8518=CARTESIAN_POINT('Ctrl Pts',(1.4878169858378,12.2395319201809,-1.3423990056639));
#8519=CARTESIAN_POINT('Ctrl Pts',(1.52583806566909,12.262545746787,-1.29900653940983));
#8520=CARTESIAN_POINT('Ctrl Pts',(1.5618016703216,12.2853161301975,-1.25422343601351));
#8521=CARTESIAN_POINT('Ctrl Pts',(1.59776527497412,12.3080865136081,-1.2094403326172));
#8522=CARTESIAN_POINT('Ctrl Pts',(1.63167113305352,12.3306131725868,-1.16326733827348));
#8523=CARTESIAN_POINT('Ctrl Pts',(1.66338758908114,12.3527790887189,-1.11599400238341));
#8524=CARTESIAN_POINT('Ctrl Pts',(1.6678334659181,12.3558862118166,-1.10936742881995));
#8525=CARTESIAN_POINT('Ctrl Pts',(1.67223640644802,12.3589862646408,-1.10271926064603));
#8526=CARTESIAN_POINT('Ctrl Pts',(1.67659613043343,12.3620789434068,-1.09605031831597));
#8527=CARTESIAN_POINT('Ctrl Pts',(1.70717378629813,12.3837699649769,-1.04927657203466));
#8528=CARTESIAN_POINT('Ctrl Pts',(1.73595988153105,12.4058246274694,-1.00096226227032));
#8529=CARTESIAN_POINT('Ctrl Pts',(1.76274746586913,12.428133304787,-0.95132657717363));
#8530=CARTESIAN_POINT('Ctrl Pts',(1.78949886307494,12.4504118454918,-0.901757944524793));
#8531=CARTESIAN_POINT('Ctrl Pts',(1.81425661023879,12.4729434627398,-0.850871989765756));
#8532=CARTESIAN_POINT('Ctrl Pts',(1.83685166290801,12.4956101450068,-0.798922307447371));
#8533=CARTESIAN_POINT('Ctrl Pts',(1.85972419431202,12.5185551856565,-0.746334656617319));
#8534=CARTESIAN_POINT('Ctrl Pts',(1.88038006398497,12.541638342878,-0.692657569319742));
#8535=CARTESIAN_POINT('Ctrl Pts',(1.8986901225964,12.5647322103524,-0.638182343237275));
#8536=CARTESIAN_POINT('Ctrl Pts',(1.91677450018556,12.5875414338653,-0.584378552728654));
#8537=CARTESIAN_POINT('Ctrl Pts',(1.93257038953987,12.6103608021586,-0.529796922528835));
#8538=CARTESIAN_POINT('Ctrl Pts',(1.94600287774627,12.6330671741721,-0.474735383838342));
#8539=CARTESIAN_POINT('Ctrl Pts',(1.95968680875091,12.6561985868504,-0.418643147994041));
#8540=CARTESIAN_POINT('Ctrl Pts',(1.9709177966365,12.6792124134557,-0.36205362997159));
#8541=CARTESIAN_POINT('Ctrl Pts',(1.97967164017866,12.7019827968653,-0.305288522445932));
#8542=CARTESIAN_POINT('Ctrl Pts',(1.98842548372083,12.724753180275,-0.248523414920275));
#8543=CARTESIAN_POINT('Ctrl Pts',(1.99470232098261,12.7472798392529,-0.191583499812266));
#8544=CARTESIAN_POINT('Ctrl Pts',(1.99853290967546,12.7694457553842,-0.134785361998167));
#8545=CARTESIAN_POINT('Ctrl Pts',(1.99906986517673,12.7725528784824,-0.126823642532455));
#8546=CARTESIAN_POINT('Ctrl Pts',(1.99955883944012,12.775652931307,-0.118864689739083));
#8547=CARTESIAN_POINT('Ctrl Pts',(2.00000000000001,12.7787456100735,-0.110909354270942));
#8548=CARTESIAN_POINT('Ctrl Pts',(2.00309415362581,12.8004366316398,-0.0551132738386595));
#8549=CARTESIAN_POINT('Ctrl Pts',(2.00386648849138,12.8224912941283,0.00112119338997931));
#8550=CARTESIAN_POINT('Ctrl Pts',(2.00224737448696,12.8447999714419,0.0575007497769627));
#8551=CARTESIAN_POINT('Ctrl Pts',(2.00063044773012,12.8670785121497,0.113804143492278));
#8552=CARTESIAN_POINT('Ctrl Pts',(1.99662830833494,12.8896101294007,0.170251546599096));
#8553=CARTESIAN_POINT('Ctrl Pts',(1.99022135678646,12.9122768116708,0.22653881754767));
#8554=CARTESIAN_POINT('Ctrl Pts',(1.98373572461622,12.935221852321,0.283517324795138));
#8555=CARTESIAN_POINT('Ctrl Pts',(1.97478568884141,12.958305009543,0.340330980833699));
#8556=CARTESIAN_POINT('Ctrl Pts',(1.96340505170229,12.9813988770179,0.396662939804991));
#8557=CARTESIAN_POINT('Ctrl Pts',(1.95216468685348,13.0042081005275,0.45230057799216));
#8558=CARTESIAN_POINT('Ctrl Pts',(1.93855351321208,13.0270274688176,0.507467600994751));
#8559=CARTESIAN_POINT('Ctrl Pts',(1.92265561989256,13.049733840828,0.561868536368022));
#8560=CARTESIAN_POINT('Ctrl Pts',(1.90646013384314,13.0728652535087,0.617287803072458));
#8561=CARTESIAN_POINT('Ctrl Pts',(1.88789169564903,13.0958790801163,0.671911257216334));
#8562=CARTESIAN_POINT('Ctrl Pts',(1.8670901927726,13.1186494635283,0.725448204158746));
#8563=CARTESIAN_POINT('Ctrl Pts',(1.84628868989617,13.1414198469403,0.77898515110116));
#8564=CARTESIAN_POINT('Ctrl Pts',(1.82325463286394,13.1639465059205,0.831434982710294));
#8565=CARTESIAN_POINT('Ctrl Pts',(1.79817295107358,13.186112422054,0.882538907296488));
#8566=CARTESIAN_POINT('Ctrl Pts',(1.79465710844671,13.1892195451511,0.889702436359735));
#8567=CARTESIAN_POINT('Ctrl Pts',(1.79110109618515,13.1923195979747,0.896839578795523));
#8568=CARTESIAN_POINT('Ctrl Pts',(1.78750548470433,13.1954122767401,0.903949681684049));
#8569=CARTESIAN_POINT('Ctrl Pts',(1.76228706012136,13.217103298315,0.95381758160267));
#8570=CARTESIAN_POINT('Ctrl Pts',(1.73483868810907,13.2391579608124,1.00290422624289));
#8571=CARTESIAN_POINT('Ctrl Pts',(1.70524671604273,13.261466638135,1.05092079734406));
#8572=CARTESIAN_POINT('Ctrl Pts',(1.67569471954095,13.2837451788392,1.09887250323334));
#8573=CARTESIAN_POINT('Ctrl Pts',(1.64400506360599,13.3062767960864,1.14575631859508));
#8574=CARTESIAN_POINT('Ctrl Pts',(1.61031284533477,13.3289434783527,1.1912990493636));
#8575=CARTESIAN_POINT('Ctrl Pts',(1.57620686949313,13.3518885190016,1.23740106802114));
#8576=CARTESIAN_POINT('Ctrl Pts',(1.54004908312944,13.3749716762223,1.28212811954181));
#8577=CARTESIAN_POINT('Ctrl Pts',(1.5020271827717,13.3980655436958,1.32522270848326));
#8578=CARTESIAN_POINT('Ctrl Pts',(1.46447392217234,13.4208747672044,1.36778613413307));
#8579=CARTESIAN_POINT('Ctrl Pts',(1.42510278852357,13.4436941354935,1.40875659068142));
#8580=CARTESIAN_POINT('Ctrl Pts',(1.38413434135706,13.4664005075029,1.44792023604233));
#8581=CARTESIAN_POINT('Ctrl Pts',(1.34239900566176,13.489531920182,1.48781698583969));
#8582=CARTESIAN_POINT('Ctrl Pts',(1.29900653940771,13.5125457467881,1.52583806567085));
#8583=CARTESIAN_POINT('Ctrl Pts',(1.25422343601143,13.5353161301986,1.56180167032324));
#8584=CARTESIAN_POINT('Ctrl Pts',(1.20944033261515,13.5580865136091,1.59776527497563));
#8585=CARTESIAN_POINT('Ctrl Pts',(1.16326733827152,13.5806131725877,1.63167113305488));
#8586=CARTESIAN_POINT('Ctrl Pts',(1.11599400238149,13.6027790887198,1.66338758908239));
#8587=CARTESIAN_POINT('Ctrl Pts',(1.10936742881865,13.6058862118172,1.66783346591892));
#8588=CARTESIAN_POINT('Ctrl Pts',(1.1027192606454,13.6089862646411,1.6722364064484));
#8589=CARTESIAN_POINT('Ctrl Pts',(1.09605031831597,13.6120789434068,1.67659613043339));
#8590=CARTESIAN_POINT('Ctrl Pts',(1.04927657204321,13.6337699649729,1.7071737862925));
#8591=CARTESIAN_POINT('Ctrl Pts',(1.00096226228807,13.6558246274613,1.73595988152044));
#8592=CARTESIAN_POINT('Ctrl Pts',(0.951326577201009,13.6781333047747,1.76274746585431));
#8593=CARTESIAN_POINT('Ctrl Pts',(0.901757944547673,13.7004118454817,1.78949886306355));
#8594=CARTESIAN_POINT('Ctrl Pts',(0.850871989783864,13.7229434627318,1.81425661023042));
#8595=CARTESIAN_POINT('Ctrl Pts',(0.798922307460442,13.7456101450011,1.83685166290228));
#8596=CARTESIAN_POINT('Ctrl Pts',(0.746334656629352,13.7685551856513,1.85972419430719));
#8597=CARTESIAN_POINT('Ctrl Pts',(0.692657569330676,13.7916383428733,1.88038006398094));
#8598=CARTESIAN_POINT('Ctrl Pts',(0.638182343247026,13.8147322103483,1.89869012259308));
#8599=CARTESIAN_POINT('Ctrl Pts',(0.584378552748106,13.837541433857,1.91677450017928));
#8600=CARTESIAN_POINT('Ctrl Pts',(0.52979692255822,13.8603608021463,1.93257038953147));
#8601=CARTESIAN_POINT('Ctrl Pts',(0.474735383877795,13.8830671741558,1.94600287773661));
#8602=CARTESIAN_POINT('Ctrl Pts',(0.418643148026858,13.906198586837,1.95968680874406));
#8603=CARTESIAN_POINT('Ctrl Pts',(0.362053629997598,13.9292124134452,1.97091779663188));
#8604=CARTESIAN_POINT('Ctrl Pts',(0.305288522465042,13.9519827968577,1.97967164017568));
#8605=CARTESIAN_POINT('Ctrl Pts',(0.248523414932487,13.9747531802702,1.98842548371947));
#8606=CARTESIAN_POINT('Ctrl Pts',(0.191583499817506,13.9972798392508,1.99470232098228));
#8607=CARTESIAN_POINT('Ctrl Pts',(0.134785361996449,14.0194457553848,1.99853290967556));
#8608=CARTESIAN_POINT('Ctrl Pts',(0.126823642531306,14.0225528784828,1.99906986517678));
#8609=CARTESIAN_POINT('Ctrl Pts',(0.118864689738491,14.0256529313072,1.99955883944013));
#8610=CARTESIAN_POINT('Ctrl Pts',(0.110909354270912,14.0287456100735,1.99999999999999));
#8611=CARTESIAN_POINT('Ctrl Pts',(0.0551132738272201,14.0504366316442,2.00309415362644));
#8612=CARTESIAN_POINT('Ctrl Pts',(-0.00112119341301478,14.0724912941373,
2.00386648849169));
#8613=CARTESIAN_POINT('Ctrl Pts',(-0.0575007498115822,14.0947999714556,
2.00224737448596));
#8614=CARTESIAN_POINT('Ctrl Pts',(-0.113804143535633,14.1170785121669,2.0006304477279));
#8615=CARTESIAN_POINT('Ctrl Pts',(-0.170251546651125,14.1396101294215,1.99662830833074));
#8616=CARTESIAN_POINT('Ctrl Pts',(-0.226538817608238,14.1622768116952,1.99022135677956));
#8617=CARTESIAN_POINT('Ctrl Pts',(-0.283517324850062,14.1852218523432,1.9837357246082));
#8618=CARTESIAN_POINT('Ctrl Pts',(-0.340330980882965,14.2083050095631,1.97478568883275));
#8619=CARTESIAN_POINT('Ctrl Pts',(-0.396662939848583,14.2313988770357,1.96340505169347));
#8620=CARTESIAN_POINT('Ctrl Pts',(-0.452300578033097,14.2542081005444,1.95216468684391));
#8621=CARTESIAN_POINT('Ctrl Pts',(-0.507467601032979,14.2770274688335,1.93855351320199));
#8622=CARTESIAN_POINT('Ctrl Pts',(-0.561868536403543,14.2997338408429,1.92265561988216));
#8623=CARTESIAN_POINT('Ctrl Pts',(-0.617287803100842,14.3228652535207,1.90646013383371));
#8624=CARTESIAN_POINT('Ctrl Pts',(-0.671911257237724,14.3458790801254,1.88789169564117));
#8625=CARTESIAN_POINT('Ctrl Pts',(-0.725448204173397,14.3686494635346,1.86709019276687));
#8626=CARTESIAN_POINT('Ctrl Pts',(-0.778985151109067,14.3914198469438,1.84628868989257));
#8627=CARTESIAN_POINT('Ctrl Pts',(-0.831434982711695,14.4139465059212,1.82325463286305));
#8628=CARTESIAN_POINT('Ctrl Pts',(-0.882538907291681,14.436112422052,1.79817295107591));
#8629=CARTESIAN_POINT('Ctrl Pts',(-0.889702436356552,14.4392195451498,1.79465710844826));
#8630=CARTESIAN_POINT('Ctrl Pts',(-0.896839578793936,14.4423195979741,1.79110109618591));
#8631=CARTESIAN_POINT('Ctrl Pts',(-0.903949681684057,14.4454122767402,1.78750548470429));
#8632=CARTESIAN_POINT('Ctrl Pts',(-0.953817581601736,14.4671032983147,1.7622870601218));
#8633=CARTESIAN_POINT('Ctrl Pts',(-1.00290422624106,14.4891579608116,1.73483868811007));
#8634=CARTESIAN_POINT('Ctrl Pts',(-1.05092079734141,14.5114666381338,1.70524671604434));
#8635=CARTESIAN_POINT('Ctrl Pts',(-1.09887250323354,14.5337451788393,1.67569471954091));
#8636=CARTESIAN_POINT('Ctrl Pts',(-1.14575631859805,14.5562767960879,1.64400506360401));
#8637=CARTESIAN_POINT('Ctrl Pts',(-1.19129904936917,14.5789434783555,1.61031284533064));
#8638=CARTESIAN_POINT('Ctrl Pts',(-1.23740106802587,14.6018885190041,1.57620686948938));
#8639=CARTESIAN_POINT('Ctrl Pts',(-1.28212811954568,14.6249716762243,1.54004908312616));
#8640=CARTESIAN_POINT('Ctrl Pts',(-1.32522270848637,14.6480655436975,1.50202718276894));
#8641=CARTESIAN_POINT('Ctrl Pts',(-1.36778613413622,14.6708747672062,1.46447392216936));
#8642=CARTESIAN_POINT('Ctrl Pts',(-1.40875659068459,14.6936941354953,1.42510278852042));
#8643=CARTESIAN_POINT('Ctrl Pts',(-1.44792023604552,14.7164005075047,1.38413434135369));
#8644=CARTESIAN_POINT('Ctrl Pts',(-1.48781698584175,14.7395319201833,1.34239900565937));
#8645=CARTESIAN_POINT('Ctrl Pts',(-1.52583806567186,14.7625457467887,1.29900653940642));
#8646=CARTESIAN_POINT('Ctrl Pts',(-1.56180167032331,14.7853161301986,1.2542234360113));
#8647=CARTESIAN_POINT('Ctrl Pts',(-1.59776527497476,14.8080865136085,1.20944033261618));
#8648=CARTESIAN_POINT('Ctrl Pts',(-1.63167113305322,14.8306131725866,1.16326733827374));
#8649=CARTESIAN_POINT('Ctrl Pts',(-1.66338758908002,14.8527790887181,1.11599400238499));
#8650=CARTESIAN_POINT('Ctrl Pts',(-1.66783346591735,14.8558862118161,1.10936742882098));
#8651=CARTESIAN_POINT('Ctrl Pts',(-1.67223640644763,14.8589862646405,1.10271926064654));
#8652=CARTESIAN_POINT('Ctrl Pts',(-1.67659613043341,14.8620789434068,1.09605031831592));
#8653=CARTESIAN_POINT('Ctrl Pts',(-1.70717378629289,14.8837699649732,1.04927657204259));
#8654=CARTESIAN_POINT('Ctrl Pts',(-1.73595988152119,14.9058246274618,1.00096226228679));
#8655=CARTESIAN_POINT('Ctrl Pts',(-1.76274746585537,14.9281333047756,0.951326577199046));
#8656=CARTESIAN_POINT('Ctrl Pts',(-1.78949886307631,14.9504118454923,0.901757944523873));
#8657=CARTESIAN_POINT('Ctrl Pts',(-1.81425661025313,14.9729434627525,0.850871989737085));
#8658=CARTESIAN_POINT('Ctrl Pts',(-1.83685166293298,14.9956101450319,0.798922307389847));
#8659=CARTESIAN_POINT('Ctrl Pts',(-1.85972419433329,15.0185551856796,0.746334656563815));
#8660=CARTESIAN_POINT('Ctrl Pts',(-1.88038006400286,15.041638342899,0.692657569270616));
#8661=CARTESIAN_POINT('Ctrl Pts',(-1.89869012261134,15.0647322103713,0.638182343192682));
#8662=CARTESIAN_POINT('Ctrl Pts',(-1.9167745001939,15.0875414338774,0.584378552699522));
#8663=CARTESIAN_POINT('Ctrl Pts',(-1.93257038954294,15.110360802164,0.529796922515685));
#8664=CARTESIAN_POINT('Ctrl Pts',(-1.94600287774547,15.1330671741708,0.474735383841463));
#8665=CARTESIAN_POINT('Ctrl Pts',(-1.95968680875032,15.1561985868493,0.418643147996668));
#8666=CARTESIAN_POINT('Ctrl Pts',(-1.97091779663606,15.1792124134548,0.362053629973788));
#8667=CARTESIAN_POINT('Ctrl Pts',(-1.97967164017836,15.2019827968646,0.305288522447653));
#8668=CARTESIAN_POINT('Ctrl Pts',(-1.98842548372065,15.2247531802745,0.248523414921518));
#8669=CARTESIAN_POINT('Ctrl Pts',(-1.99470232098253,15.2472798392525,0.191583499813044));
#8670=CARTESIAN_POINT('Ctrl Pts',(-1.99853290967543,15.269445755384,0.134785361998419));
#8671=CARTESIAN_POINT('Ctrl Pts',(-1.9990698651767,15.2725528784823,0.126823642532606));
#8672=CARTESIAN_POINT('Ctrl Pts',(-1.9995588394401,15.2756529313069,0.118864689739133));
#8673=CARTESIAN_POINT('Ctrl Pts',(-2.,15.2787456100735,0.110909354270892));
#8674=CARTESIAN_POINT('Ctrl Pts',(-2.0030941536263,15.3004366316433,0.0551132738295713));
#8675=CARTESIAN_POINT('Ctrl Pts',(-2.00386648849161,15.3224912941354,-0.0011211934082543));
#8676=CARTESIAN_POINT('Ctrl Pts',(-2.00224737448615,15.3447999714527,-0.0575007498044029));
#8677=CARTESIAN_POINT('Ctrl Pts',(-2.00063044772843,15.3670785121621,-0.113804143523693));
#8678=CARTESIAN_POINT('Ctrl Pts',(-1.99662830833203,15.3896101294147,-0.170251546634409));
#8679=CARTESIAN_POINT('Ctrl Pts',(-1.99022135678199,15.4122768116865,-0.226538817586818));
#8680=CARTESIAN_POINT('Ctrl Pts',(-1.98373572461104,15.4352218523353,-0.28351732483059));
#8681=CARTESIAN_POINT('Ctrl Pts',(-1.97478568883582,15.4583050095559,-0.340330980865487));
#8682=CARTESIAN_POINT('Ctrl Pts',(-1.96340505169662,15.4813988770293,-0.396662939833066));
#8683=CARTESIAN_POINT('Ctrl Pts',(-1.95216468684707,15.5042081005389,-0.452300578019836));
#8684=CARTESIAN_POINT('Ctrl Pts',(-1.93855351320496,15.5270274688289,-0.507467601021982));
#8685=CARTESIAN_POINT('Ctrl Pts',(-1.92265561988476,15.5497338408392,-0.561868536394774));
#8686=CARTESIAN_POINT('Ctrl Pts',(-1.90646013383607,15.5728652535177,-0.61728780309387));
#8687=CARTESIAN_POINT('Ctrl Pts',(-1.88789169564315,15.5958790801231,-0.671911257232479));
#8688=CARTESIAN_POINT('Ctrl Pts',(-1.86709019276833,15.618649463533,-0.725448204169802));
#8689=CARTESIAN_POINT('Ctrl Pts',(-1.84628868989351,15.6414198469429,-0.778985151107124));
#8690=CARTESIAN_POINT('Ctrl Pts',(-1.82325463286332,15.6639465059209,-0.831434982711367));
#8691=CARTESIAN_POINT('Ctrl Pts',(-1.79817295107539,15.6861124220524,-0.882538907292868));
#8692=CARTESIAN_POINT('Ctrl Pts',(-1.79465710844794,15.6892195451501,-0.889702436357341));
#8693=CARTESIAN_POINT('Ctrl Pts',(-1.79110109618575,15.6923195979742,-0.896839578794375));
#8694=CARTESIAN_POINT('Ctrl Pts',(-1.78750548470433,15.6954122767401,-0.90394968168411));
#8695=CARTESIAN_POINT('Ctrl Pts',(-1.76228694372129,15.7171033984337,-0.953817811776782));
#8696=CARTESIAN_POINT('Ctrl Pts',(-1.7348384346849,15.7391581644147,-1.00290467937114));
#8697=CARTESIAN_POINT('Ctrl Pts',(-1.70524630628172,15.7614669470439,-1.05092146223084));
#8698=CARTESIAN_POINT('Ctrl Pts',(-1.67569381899318,15.7837458452052,-1.09887392262047));
#8699=CARTESIAN_POINT('Ctrl Pts',(-1.64400360450942,15.8062778274659,-1.14575845707494));
#8700=CARTESIAN_POINT('Ctrl Pts',(-1.6103107669867,15.8289448765748,-1.19130185872078));
#8701=CARTESIAN_POINT('Ctrl Pts',(-1.57500230505964,15.8526988462403,-1.23902913790753));
#8702=CARTESIAN_POINT('Ctrl Pts',(-1.53749452927016,15.876600854243,-1.28528257992073));
#8703=CARTESIAN_POINT('Ctrl Pts',(-1.49799656462519,15.9005094948716,-1.32977711562351));
#8704=CARTESIAN_POINT('Ctrl Pts',(-1.46031104530288,15.9233210383646,-1.3722299280668));
#8705=CARTESIAN_POINT('Ctrl Pts',(-1.42081463632739,15.9461382987637,-1.41308123426202));
#8706=CARTESIAN_POINT('Ctrl Pts',(-1.37972921806466,15.9688381759537,-1.45211851089488));
#8707=CARTESIAN_POINT('Ctrl Pts',(-1.33864416295559,15.9915378524997,-1.49115544247757));
#8708=CARTESIAN_POINT('Ctrl Pts',(-1.29597073421029,16.0141198611299,-1.52837796258682));
#8709=CARTESIAN_POINT('Ctrl Pts',(-1.25196176236387,16.0364652934131,-1.56361524373601));
#8710=CARTESIAN_POINT('Ctrl Pts',(-1.20788630186401,16.058844485124,-1.5989057612885));
#8711=CARTESIAN_POINT('Ctrl Pts',(-1.16247193926722,16.0809861259264,-1.63220477934516));
#8712=CARTESIAN_POINT('Ctrl Pts',(-1.11599400092916,16.1027790894007,-1.66338759005681));
#8713=CARTESIAN_POINT('Ctrl Pts',(-1.10936742784726,16.1058862122702,-1.66783346656228));
#8714=CARTESIAN_POINT('Ctrl Pts',(-1.10271926015816,16.108986264867,-1.67223640676696));
#8715=CARTESIAN_POINT('Ctrl Pts',(-1.09605031831592,16.1120789434068,-1.67659613043346));
#8716=CARTESIAN_POINT('Ctrl Pts',(-1.04927657203949,16.1337699649747,-1.70717378629496));
#8717=CARTESIAN_POINT('Ctrl Pts',(-1.00096226228034,16.1558246274648,-1.73595988152507));
#8718=CARTESIAN_POINT('Ctrl Pts',(-0.951326577189098,16.17813330478,-1.76274746586078));
#8719=CARTESIAN_POINT('Ctrl Pts',(-0.901757944534647,16.2004118454875,-1.78949886307018));
#8720=CARTESIAN_POINT('Ctrl Pts',(-0.850871989769685,16.2229434627381,-1.81425661023715));
#8721=CARTESIAN_POINT('Ctrl Pts',(-0.798922307445119,16.2456101450078,-1.83685166290899));
#8722=CARTESIAN_POINT('Ctrl Pts',(-0.746334656615035,16.2685551856575,-1.85972419431294));
#8723=CARTESIAN_POINT('Ctrl Pts',(-0.69265756931742,16.291638342879,-1.88038006398583));
#8724=CARTESIAN_POINT('Ctrl Pts',(-0.638182343234895,16.3147322103534,-1.89869012259721));
#8725=CARTESIAN_POINT('Ctrl Pts',(-0.584378552734248,16.3375414338629,-1.91677450018361));
#8726=CARTESIAN_POINT('Ctrl Pts',(-0.52979692254261,16.3603608021528,-1.93257038953586));
#8727=CARTESIAN_POINT('Ctrl Pts',(-0.474735383860447,16.383067174163,-1.9460028777409));
#8728=CARTESIAN_POINT('Ctrl Pts',(-0.41864314801215,16.406198586843,-1.95968680874718));
#8729=CARTESIAN_POINT('Ctrl Pts',(-0.362053629985638,16.42921241345,-1.97091779663406));
#8730=CARTESIAN_POINT('Ctrl Pts',(-0.305288522455835,16.4519827968614,-1.97967164017715));
#8731=CARTESIAN_POINT('Ctrl Pts',(-0.248523414926033,16.4747531802727,-1.98842548372025));
#8732=CARTESIAN_POINT('Ctrl Pts',(-0.191583499813838,16.4972798392523,-1.99470232098261));
#8733=CARTESIAN_POINT('Ctrl Pts',(-0.134785361995554,16.5194457553852,-1.99853290967566));
#8734=CARTESIAN_POINT('Ctrl Pts',(-0.126823642530709,16.522552878483,-1.99906986517686));
#8735=CARTESIAN_POINT('Ctrl Pts',(-0.118864689738204,16.5256529313073,-1.99955883944019));
#8736=CARTESIAN_POINT('Ctrl Pts',(-0.110909354270924,16.5287456100735,-2.00000000000003));
#8737=CARTESIAN_POINT('Ctrl Pts',(-0.0551132738242786,16.5504366316454,
-2.00309415362662));
#8738=CARTESIAN_POINT('Ctrl Pts',(0.00112119341897333,16.5724912941397,
-2.00386648849178));
#8739=CARTESIAN_POINT('Ctrl Pts',(0.0575007498205267,16.5947999714591,-2.00224737448572));
#8740=CARTESIAN_POINT('Ctrl Pts',(0.113804143545222,16.6170785121707,-2.00063044772738));
#8741=CARTESIAN_POINT('Ctrl Pts',(0.170251546661352,16.6396101294255,-1.99662830832989));
#8742=CARTESIAN_POINT('Ctrl Pts',(0.226538817619078,16.6622768116995,-1.99022135677833));
#8743=CARTESIAN_POINT('Ctrl Pts',(0.283517324860016,16.6852218523473,-1.98373572460676));
#8744=CARTESIAN_POINT('Ctrl Pts',(0.340330980892024,16.7083050095667,-1.97478568883116));
#8745=CARTESIAN_POINT('Ctrl Pts',(0.396662939856765,16.7313988770391,-1.96340505169182));
#8746=CARTESIAN_POINT('Ctrl Pts',(0.452300578040149,16.7542081005473,-1.95216468684225));
#8747=CARTESIAN_POINT('Ctrl Pts',(0.507467601038886,16.7770274688359,-1.93855351320042));
#8748=CARTESIAN_POINT('Ctrl Pts',(0.56186853640834,16.7997338408448,-1.92265561988078));
#8749=CARTESIAN_POINT('Ctrl Pts',(0.617287803104898,16.8228652535224,-1.9064601338324));
#8750=CARTESIAN_POINT('Ctrl Pts',(0.671911257241057,16.8458790801268,-1.88789169564));
#8751=CARTESIAN_POINT('Ctrl Pts',(0.725448204175984,16.8686494635356,-1.86709019276591));
#8752=CARTESIAN_POINT('Ctrl Pts',(0.778985151110912,16.8914198469445,-1.84628868989182));
#8753=CARTESIAN_POINT('Ctrl Pts',(0.831434982712801,16.9139465059216,-1.82325463286257));
#8754=CARTESIAN_POINT('Ctrl Pts',(0.882538907292112,16.9361124220521,-1.79817295107574));
#8755=CARTESIAN_POINT('Ctrl Pts',(0.889702436356832,16.9392195451499,-1.79465710844817));
#8756=CARTESIAN_POINT('Ctrl Pts',(0.89683957879411,16.942319597974,-1.79110109618587));
#8757=CARTESIAN_POINT('Ctrl Pts',(0.903949681684087,16.9454122767401,-1.78750548470432));
#8758=CARTESIAN_POINT('Ctrl Pts',(0.953817581597555,16.9671032983128,-1.76228706012394));
#8759=CARTESIAN_POINT('Ctrl Pts',(1.00290422623283,16.9891579608078,-1.73483868811471));
#8760=CARTESIAN_POINT('Ctrl Pts',(1.05092079732929,17.0114666381281,-1.70524671605184));
#8761=CARTESIAN_POINT('Ctrl Pts',(1.09887250324054,17.0337451788424,-1.67569471953709));
#8762=CARTESIAN_POINT('Ctrl Pts',(1.14575631862329,17.0562767960999,-1.64400506358722));
#8763=CARTESIAN_POINT('Ctrl Pts',(1.19129904941155,17.0789434783766,-1.61031284529931));
#8764=CARTESIAN_POINT('Ctrl Pts',(1.23740106806408,17.1018885190235,-1.57620686945925));
#8765=CARTESIAN_POINT('Ctrl Pts',(1.28212811957984,17.1249716762422,-1.5400490830976));
#8766=CARTESIAN_POINT('Ctrl Pts',(1.32522270851665,17.1480655437137,-1.50202718274225));
#8767=CARTESIAN_POINT('Ctrl Pts',(1.36778613416616,17.1708747672226,-1.46447392214146));
#8768=CARTESIAN_POINT('Ctrl Pts',(1.40875659071413,17.193694135512,-1.42510278849127));
#8769=CARTESIAN_POINT('Ctrl Pts',(1.44792023607454,17.2164005075216,-1.38413434132337));
#8770=CARTESIAN_POINT('Ctrl Pts',(1.4878169858654,17.2395319201974,-1.34239900563293));
#8771=CARTESIAN_POINT('Ctrl Pts',(1.52583806569053,17.2625457468003,-1.29900653938427));
#8772=CARTESIAN_POINT('Ctrl Pts',(1.56180167033742,17.2853161302076,-1.25422343599379));
#8773=CARTESIAN_POINT('Ctrl Pts',(1.59776527498432,17.3080865136148,-1.20944033260332));
#8774=CARTESIAN_POINT('Ctrl Pts',(1.63167113305864,17.3306131725904,-1.16326733826587));
#8775=CARTESIAN_POINT('Ctrl Pts',(1.66338758908179,17.3527790887194,-1.11599400238241));
#8776=CARTESIAN_POINT('Ctrl Pts',(1.66783346591852,17.3558862118169,-1.10936742881929));
#8777=CARTESIAN_POINT('Ctrl Pts',(1.6722364064482,17.3589862646409,-1.10271926064573));
#8778=CARTESIAN_POINT('Ctrl Pts',(1.6765961304334,17.3620789434068,-1.09605031831599));
#8779=CARTESIAN_POINT('Ctrl Pts',(1.70717378629827,17.3837699649771,-1.04927657203438));
#8780=CARTESIAN_POINT('Ctrl Pts',(1.73595988153134,17.4058246274697,-1.00096226226976));
#8781=CARTESIAN_POINT('Ctrl Pts',(1.76274746586953,17.4281333047874,-0.951326577172805));
#8782=CARTESIAN_POINT('Ctrl Pts',(1.78949886307612,17.4504118454929,-0.901757944522451));
#8783=CARTESIAN_POINT('Ctrl Pts',(1.81425661024061,17.4729434627415,-0.850871989761866));
#8784=CARTESIAN_POINT('Ctrl Pts',(1.83685166291036,17.4956101450092,-0.798922307441834));
#8785=CARTESIAN_POINT('Ctrl Pts',(1.8597241943142,17.5185551856589,-0.746334656611749));
#8786=CARTESIAN_POINT('Ctrl Pts',(1.88038006398696,17.5416383428804,-0.692657569314163));
#8787=CARTESIAN_POINT('Ctrl Pts',(1.89869012259822,17.5647322103548,-0.638182343231689));
#8788=CARTESIAN_POINT('Ctrl Pts',(1.9167745001822,17.5875414338613,-0.584378552737978));
#8789=CARTESIAN_POINT('Ctrl Pts',(1.93257038953261,17.6103608021483,-0.529796922553466));
#8790=CARTESIAN_POINT('Ctrl Pts',(1.94600287773644,17.6330671741555,-0.474735383878508));
#8791=CARTESIAN_POINT('Ctrl Pts',(1.95968680874409,17.656198586837,-0.418643148026851));
#8792=CARTESIAN_POINT('Ctrl Pts',(1.97091779663205,17.6792124134455,-0.362053629996861));
#8793=CARTESIAN_POINT('Ctrl Pts',(1.97967164017591,17.7019827968583,-0.305288522463581));
#8794=CARTESIAN_POINT('Ctrl Pts',(1.98842548371977,17.7247531802711,-0.248523414930299));
#8795=CARTESIAN_POINT('Ctrl Pts',(1.9947023209826,17.747279839252,-0.191583499814546));
#8796=CARTESIAN_POINT('Ctrl Pts',(1.99853290967582,17.7694457553863,-0.134785361992776));
#8797=CARTESIAN_POINT('Ctrl Pts',(1.99906986517694,17.7725528784838,-0.126823642528859));
#8798=CARTESIAN_POINT('Ctrl Pts',(1.99955883944021,17.7756529313077,-0.118864689737281));
#8799=CARTESIAN_POINT('Ctrl Pts',(2.,17.7787456100735,-0.110909354270934));
#8800=CARTESIAN_POINT('Ctrl Pts',(2.003094153626,17.8004366316412,-0.0551132738349501));
#8801=CARTESIAN_POINT('Ctrl Pts',(2.00386648849147,17.8224912941312,0.00112119339748048));
#8802=CARTESIAN_POINT('Ctrl Pts',(2.00224737448663,17.8447999714463,0.0575007497882499));
#8803=CARTESIAN_POINT('Ctrl Pts',(2.00063044772936,17.8670785121557,0.113804143507444));
#8804=CARTESIAN_POINT('Ctrl Pts',(1.99662830833342,17.8896101294083,0.170251546618121));
#8805=CARTESIAN_POINT('Ctrl Pts',(1.99022135678385,17.91227681168,0.226538817570541));
#8806=CARTESIAN_POINT('Ctrl Pts',(1.98373572461321,17.9352218523293,0.283517324815695));
#8807=CARTESIAN_POINT('Ctrl Pts',(1.97478568883819,17.9583050095504,0.340330980851915));
#8808=CARTESIAN_POINT('Ctrl Pts',(1.96340505169907,17.9813988770244,0.396662939820889));
#8809=CARTESIAN_POINT('Ctrl Pts',(1.95216468685023,18.0042081005331,0.452300578005842));
#8810=CARTESIAN_POINT('Ctrl Pts',(1.93855351320902,18.0270274688224,0.507467601006192));
#8811=CARTESIAN_POINT('Ctrl Pts',(1.92265561988986,18.0497338408319,0.561868536377263));
#8812=CARTESIAN_POINT('Ctrl Pts',(1.90646013384083,18.0728652535116,0.617287803079352));
#8813=CARTESIAN_POINT('Ctrl Pts',(1.88789169564731,18.0958790801183,0.671911257220936));
#8814=CARTESIAN_POINT('Ctrl Pts',(1.86709019277166,18.1186494635294,0.725448204161157));
#8815=CARTESIAN_POINT('Ctrl Pts',(1.846288689896,18.1414198469404,0.778985151101378));
#8816=CARTESIAN_POINT('Ctrl Pts',(1.82325463286474,18.1639465059197,0.831434982708388));
#8817=CARTESIAN_POINT('Ctrl Pts',(1.79817295107552,18.1861124220523,0.882538907292541));
#8818=CARTESIAN_POINT('Ctrl Pts',(1.79465710844803,18.18921954515,0.889702436357106));
#8819=CARTESIAN_POINT('Ctrl Pts',(1.79110109618581,18.1923195979741,0.896839578794223));
#8820=CARTESIAN_POINT('Ctrl Pts',(1.78750548470433,18.1954122767401,0.903949681684052));
#8821=CARTESIAN_POINT('Ctrl Pts',(1.76228706013497,18.2171032983033,0.953817581575735));
#8822=CARTESIAN_POINT('Ctrl Pts',(1.73483868813874,18.2391579607885,1.00290422618985));
#8823=CARTESIAN_POINT('Ctrl Pts',(1.70524671609067,18.2614666380988,1.05092079726627));
#8824=CARTESIAN_POINT('Ctrl Pts',(1.6756947195693,18.2837451788193,1.09887250319222));
#8825=CARTESIAN_POINT('Ctrl Pts',(1.64400506361153,18.3062767960832,1.14575631858921));
#8826=CARTESIAN_POINT('Ctrl Pts',(1.61031284531455,18.3289434783663,1.19129904939094));
#8827=CARTESIAN_POINT('Ctrl Pts',(1.57620686947382,18.3518885190141,1.23740106804561));
#8828=CARTESIAN_POINT('Ctrl Pts',(1.54004908311129,18.3749716762336,1.28212811956348));
#8829=CARTESIAN_POINT('Ctrl Pts',(1.50202718275492,18.398065543706,1.32522270850227));
#8830=CARTESIAN_POINT('Ctrl Pts',(1.46447392215565,18.4208747672142,1.36778613415087));
#8831=CARTESIAN_POINT('Ctrl Pts',(1.42510278850714,18.4436941355029,1.408756590698));
#8832=CARTESIAN_POINT('Ctrl Pts',(1.3841343413409,18.4664005075118,1.44792023605776));
#8833=CARTESIAN_POINT('Ctrl Pts',(1.34239900564798,18.4895319201894,1.48781698585197));
#8834=CARTESIAN_POINT('Ctrl Pts',(1.29900653939657,18.5125457467939,1.52583806568019));
#8835=CARTESIAN_POINT('Ctrl Pts',(1.25422343600313,18.5353161302028,1.5618016703299));
#8836=CARTESIAN_POINT('Ctrl Pts',(1.20944033260969,18.5580865136117,1.59776527497961));
#8837=CARTESIAN_POINT('Ctrl Pts',(1.16326733826908,18.5806131725888,1.63167113305647));
#8838=CARTESIAN_POINT('Ctrl Pts',(1.11599400238223,18.6027790887194,1.66338758908188));
#8839=CARTESIAN_POINT('Ctrl Pts',(1.10936742881915,18.605886211817,1.66783346591857));
#8840=CARTESIAN_POINT('Ctrl Pts',(1.10271926064563,18.608986264641,1.67223640644824));
#8841=CARTESIAN_POINT('Ctrl Pts',(1.09605031831596,18.6120789434068,1.67659613043339));
#8842=CARTESIAN_POINT('Ctrl Pts',(1.04927657203943,18.6337699649747,1.70717378629498));
#8843=CARTESIAN_POINT('Ctrl Pts',(1.00096226228026,18.6558246274649,1.73595988152509));
#8844=CARTESIAN_POINT('Ctrl Pts',(0.951326577188937,18.6781333047801,1.76274746586083));
#8845=CARTESIAN_POINT('Ctrl Pts',(0.901757944528287,18.7004118454903,1.78949886307358));
#8846=CARTESIAN_POINT('Ctrl Pts',(0.850871989756818,18.7229434627438,1.81425661024339));
#8847=CARTESIAN_POINT('Ctrl Pts',(0.798922307425478,18.7456101450164,1.83685166291751));
#8848=CARTESIAN_POINT('Ctrl Pts',(0.746334656596687,18.7685551856654,1.85972419432023));
#8849=CARTESIAN_POINT('Ctrl Pts',(0.692657569300505,18.7916383428862,1.88038006399197));
#8850=CARTESIAN_POINT('Ctrl Pts',(0.638182343219492,18.81473221036,1.89869012260234));
#8851=CARTESIAN_POINT('Ctrl Pts',(0.584378552729531,18.8375414338648,1.91677450018467));
#8852=CARTESIAN_POINT('Ctrl Pts',(0.529796922548891,18.8603608021501,1.93257038953376));
#8853=CARTESIAN_POINT('Ctrl Pts',(0.474735383877914,18.8830671741558,1.94600287773659));
#8854=CARTESIAN_POINT('Ctrl Pts',(0.418643148026724,18.9061985868371,1.9596868087441));
#8855=CARTESIAN_POINT('Ctrl Pts',(0.362053629997216,18.9292124134453,1.97091779663196));
#8856=CARTESIAN_POINT('Ctrl Pts',(0.30528852246438,18.9519827968579,1.97967164017578));
#8857=CARTESIAN_POINT('Ctrl Pts',(0.248523414931543,18.9747531802706,1.9884254837196));
#8858=CARTESIAN_POINT('Ctrl Pts',(0.191583499816295,18.9972798392513,1.9947023209824));
#8859=CARTESIAN_POINT('Ctrl Pts',(0.134785361994945,19.0194457553854,1.99853290967565));
#8860=CARTESIAN_POINT('Ctrl Pts',(0.126823642530299,19.0225528784832,1.99906986517683));
#8861=CARTESIAN_POINT('Ctrl Pts',(0.118864689737992,19.0256529313074,1.99955883944015));
#8862=CARTESIAN_POINT('Ctrl Pts',(0.110909354270916,19.0287456100735,1.99999999999998));
#8863=CARTESIAN_POINT('Ctrl Pts',(0.0551132738329355,19.050436631642,2.00309415362612));
#8864=CARTESIAN_POINT('Ctrl Pts',(-0.00112119340150097,19.0724912941328,
2.00386648849152));
#8865=CARTESIAN_POINT('Ctrl Pts',(-0.0575007497943028,19.0947999714487,
2.00224737448645));
#8866=CARTESIAN_POINT('Ctrl Pts',(-0.113804143521595,19.1170785121613,2.00063044772879));
#8867=CARTESIAN_POINT('Ctrl Pts',(-0.170251546640372,19.1396101294171,1.99662830833176));
#8868=CARTESIAN_POINT('Ctrl Pts',(-0.226538817600756,19.1622768116922,1.99022135678042));
#8869=CARTESIAN_POINT('Ctrl Pts',(-0.283517324843176,19.1852218523405,1.98373572460921));
#8870=CARTESIAN_POINT('Ctrl Pts',(-0.340330980876671,19.2083050095605,1.97478568883386));
#8871=CARTESIAN_POINT('Ctrl Pts',(-0.396662939842893,19.2313988770334,1.96340505169463));
#8872=CARTESIAN_POINT('Ctrl Pts',(-0.452300578032891,19.2542081005443,1.95216468684413));
#8873=CARTESIAN_POINT('Ctrl Pts',(-0.507467601038136,19.2770274688356,1.93855351320081));
#8874=CARTESIAN_POINT('Ctrl Pts',(-0.561868536413931,19.2997338408472,1.92265561987913));
#8875=CARTESIAN_POINT('Ctrl Pts',(-0.617287803109304,19.3228652535242,1.90646013383092));
#8876=CARTESIAN_POINT('Ctrl Pts',(-0.671911257244324,19.3458790801282,1.88789169563878));
#8877=CARTESIAN_POINT('Ctrl Pts',(-0.725448204178154,19.3686494635366,1.86709019276504));
#8878=CARTESIAN_POINT('Ctrl Pts',(-0.778985151111984,19.3914198469451,1.8462886898913));
#8879=CARTESIAN_POINT('Ctrl Pts',(-0.831434982712839,19.4139465059217,1.82325463286249));
#8880=CARTESIAN_POINT('Ctrl Pts',(-0.882538907291128,19.4361124220518,1.7981729510762));
#8881=CARTESIAN_POINT('Ctrl Pts',(-0.889702436356173,19.4392195451497,1.79465710844847));
#8882=CARTESIAN_POINT('Ctrl Pts',(-0.896839578793776,19.442319597974,1.79110109618601));
#8883=CARTESIAN_POINT('Ctrl Pts',(-0.903949681684074,19.4454122767402,1.7875054847043));
#8884=CARTESIAN_POINT('Ctrl Pts',(-0.95381758160981,19.4671032983182,1.76228706011775));
#8885=CARTESIAN_POINT('Ctrl Pts',(-1.00290422625695,19.4891579608188,1.73483868810121));
#8886=CARTESIAN_POINT('Ctrl Pts',(-1.05092079736472,19.5114666381446,1.70524671603001));
#8887=CARTESIAN_POINT('Ctrl Pts',(-1.09887250323535,19.5337451788404,1.67569471953893));
#8888=CARTESIAN_POINT('Ctrl Pts',(-1.14575631857925,19.5562767960789,1.6440050636163));
#8889=CARTESIAN_POINT('Ctrl Pts',(-1.19129904933102,19.5789434783365,1.6103128453589));
#8890=CARTESIAN_POINT('Ctrl Pts',(-1.23740106799155,19.6018885189865,1.57620686951649));
#8891=CARTESIAN_POINT('Ctrl Pts',(-1.28212811951509,19.6249716762083,1.54004908315182));
#8892=CARTESIAN_POINT('Ctrl Pts',(-1.32522270845931,19.648065543683,1.50202718279284));
#8893=CARTESIAN_POINT('Ctrl Pts',(-1.36778613411482,19.6708747671943,1.46447392218964));
#8894=CARTESIAN_POINT('Ctrl Pts',(-1.40875659066852,19.6936941354862,1.4251027885366));
#8895=CARTESIAN_POINT('Ctrl Pts',(-1.44792023603437,19.7164005074983,1.38413434136538));
#8896=CARTESIAN_POINT('Ctrl Pts',(-1.48781698583262,19.7395319201778,1.34239900566963));
#8897=CARTESIAN_POINT('Ctrl Pts',(-1.52583806566465,19.7625457467843,1.29900653941504));
#8898=CARTESIAN_POINT('Ctrl Pts',(-1.56180167031782,19.7853161301951,1.25422343601817));
#8899=CARTESIAN_POINT('Ctrl Pts',(-1.59776527497099,19.808086513606,1.2094403326213));
#8900=CARTESIAN_POINT('Ctrl Pts',(-1.63167113305097,19.830613172585,1.16326733827702));
#8901=CARTESIAN_POINT('Ctrl Pts',(-1.66338758907914,19.8527790887175,1.11599400238632));
#8902=CARTESIAN_POINT('Ctrl Pts',(-1.66783346591677,19.8558862118157,1.10936742882188));
#8903=CARTESIAN_POINT('Ctrl Pts',(-1.67223640644734,19.8589862646403,1.10271926064701));
#8904=CARTESIAN_POINT('Ctrl Pts',(-1.67659613043341,19.8620789434068,1.09605031831594));
#8905=CARTESIAN_POINT('Ctrl Pts',(-1.7071737862944,19.8837699649743,1.04927657204031));
#8906=CARTESIAN_POINT('Ctrl Pts',(-1.73595988152403,19.905824627464,1.00096226228204));
#8907=CARTESIAN_POINT('Ctrl Pts',(-1.76274746585934,19.9281333047789,0.951326577191711));
#8908=CARTESIAN_POINT('Ctrl Pts',(-1.78949886307829,19.9504118454942,0.901757944519727));
#8909=CARTESIAN_POINT('Ctrl Pts',(-1.81425661025339,19.9729434627528,0.850871989736333));
#8910=CARTESIAN_POINT('Ctrl Pts',(-1.83685166293178,19.9956101450307,0.798922307392625));
#8911=CARTESIAN_POINT('Ctrl Pts',(-1.85972419433239,20.0185551856786,0.746334656566127));
#8912=CARTESIAN_POINT('Ctrl Pts',(-1.88038006400222,20.0416383428983,0.692657569272394));
#8913=CARTESIAN_POINT('Ctrl Pts',(-1.89869012261092,20.0647322103708,0.638182343193955));
#8914=CARTESIAN_POINT('Ctrl Pts',(-1.91677450019524,20.087541433879,0.584378552695657));
#8915=CARTESIAN_POINT('Ctrl Pts',(-1.93257038954561,20.1103608021678,0.529796922506548));
#8916=CARTESIAN_POINT('Ctrl Pts',(-1.94600287774902,20.1330671741768,0.474735383826951));
#8917=CARTESIAN_POINT('Ctrl Pts',(-1.959686808753,20.1561985868545,0.418643147983894));
#8918=CARTESIAN_POINT('Ctrl Pts',(-1.97091779663804,20.1792124134592,0.362053629962793));
#8919=CARTESIAN_POINT('Ctrl Pts',(-1.97967164017977,20.2019827968683,0.305288522438494));
#8920=CARTESIAN_POINT('Ctrl Pts',(-1.98842548372151,20.2247531802774,0.248523414914194));
#8921=CARTESIAN_POINT('Ctrl Pts',(-1.994702320983,20.2472798392547,0.191583499807577));
#8922=CARTESIAN_POINT('Ctrl Pts',(-1.99853290967566,20.2694457553854,0.134785361994836));
#8923=CARTESIAN_POINT('Ctrl Pts',(-1.99906986517684,20.2725528784832,0.126823642530228));
#8924=CARTESIAN_POINT('Ctrl Pts',(-1.99955883944016,20.2756529313074,0.118864689737925));
#8925=CARTESIAN_POINT('Ctrl Pts',(-1.99999999999999,20.2787456100735,0.110909354270875));
#8926=CARTESIAN_POINT('Ctrl Pts',(-2.00309415362675,20.3004366316465,0.0551132738212203));
#8927=CARTESIAN_POINT('Ctrl Pts',(-2.00386648849184,20.322491294142,-0.00112119342512291));
#8928=CARTESIAN_POINT('Ctrl Pts',(-2.00224737448543,20.3447999714627,-0.057500749829767));
#8929=CARTESIAN_POINT('Ctrl Pts',(-2.0006304477273,20.3670785121679,-0.113804143538167));
#8930=CARTESIAN_POINT('Ctrl Pts',(-1.99662830833143,20.3896101294162,-0.170251546637865));
#8931=CARTESIAN_POINT('Ctrl Pts',(-1.99022135678284,20.4122768116835,-0.226538817579384));
#8932=CARTESIAN_POINT('Ctrl Pts',(-1.98373572461206,20.4352218523325,-0.283517324823514));
#8933=CARTESIAN_POINT('Ctrl Pts',(-1.97478568883698,20.4583050095532,-0.340330980858763));
#8934=CARTESIAN_POINT('Ctrl Pts',(-1.9634050516979,20.4813988770268,-0.396662939826711));
#8935=CARTESIAN_POINT('Ctrl Pts',(-1.95216468684893,20.5042081005355,-0.452300578011471));
#8936=CARTESIAN_POINT('Ctrl Pts',(-1.9385535132076,20.5270274688246,-0.50746760101163));
#8937=CARTESIAN_POINT('Ctrl Pts',(-1.92265561988833,20.5497338408341,-0.561868536382517));
#8938=CARTESIAN_POINT('Ctrl Pts',(-1.90646013383956,20.5728652535133,-0.617287803083201));
#8939=CARTESIAN_POINT('Ctrl Pts',(-1.88789169564641,20.5958790801194,-0.671911257223431));
#8940=CARTESIAN_POINT('Ctrl Pts',(-1.86709019277123,20.6186494635299,-0.725448204162321));
#8941=CARTESIAN_POINT('Ctrl Pts',(-1.84628868989605,20.6414198469404,-0.778985151101207));
#8942=CARTESIAN_POINT('Ctrl Pts',(-1.8232546328654,20.6639465059191,-0.831434982706896));
#8943=CARTESIAN_POINT('Ctrl Pts',(-1.79817295107689,20.6861124220512,-0.882538907289802));
#8944=CARTESIAN_POINT('Ctrl Pts',(-1.79465710844896,20.6892195451493,-0.889702436355293));
#8945=CARTESIAN_POINT('Ctrl Pts',(-1.79110109618628,20.6923195979738,-0.896839578793339));
#8946=CARTESIAN_POINT('Ctrl Pts',(-1.78750548470434,20.6954122767402,-0.903949681684084));
#8947=CARTESIAN_POINT('Ctrl Pts',(-1.76228706012711,20.7171032983101,-0.953817581591305));
#8948=CARTESIAN_POINT('Ctrl Pts',(-1.73483868812163,20.7391579608024,-1.00290422622048));
#8949=CARTESIAN_POINT('Ctrl Pts',(-1.70524671606301,20.7614666381198,-1.05092079731117));
#8950=CARTESIAN_POINT('Ctrl Pts',(-1.67569471953583,20.7837451788437,-1.09887250324374));
#8951=CARTESIAN_POINT('Ctrl Pts',(-1.64400506357161,20.8062767961112,-1.14575631864694));
#8952=CARTESIAN_POINT('Ctrl Pts',(-1.61031284526767,20.8289434783979,-1.19129904945433));
#8953=CARTESIAN_POINT('Ctrl Pts',(-1.57620686942888,20.8518885190433,-1.23740106810258));
#8954=CARTESIAN_POINT('Ctrl Pts',(-1.54004908306881,20.8749716762603,-1.28212811961424));
#8955=CARTESIAN_POINT('Ctrl Pts',(-1.5020271827154,20.8980655437301,-1.3252227085471));
#8956=CARTESIAN_POINT('Ctrl Pts',(-1.46447392211193,20.9208747672401,-1.3677861341979));
#8957=CARTESIAN_POINT('Ctrl Pts',(-1.42510278845897,20.9436941355305,-1.40875659074693));
#8958=CARTESIAN_POINT('Ctrl Pts',(-1.38413434128816,20.9664005075411,-1.44792023610822));
#8959=CARTESIAN_POINT('Ctrl Pts',(-1.34239900560239,20.9895319202138,-1.48781698589268));
#8960=CARTESIAN_POINT('Ctrl Pts',(-1.2990065393589,21.0125457468135,-1.52583806571186));
#8961=CARTESIAN_POINT('Ctrl Pts',(-1.25422343597402,21.0353161302176,-1.56180167035333));
#8962=CARTESIAN_POINT('Ctrl Pts',(-1.20944033258914,21.0580865136218,-1.59776527499479));
#8963=CARTESIAN_POINT('Ctrl Pts',(-1.16326733825769,21.0806131725942,-1.63167113306424));
#8964=CARTESIAN_POINT('Ctrl Pts',(-1.11599400238053,21.1027790887202,-1.66338758908307));
#8965=CARTESIAN_POINT('Ctrl Pts',(-1.109367428818,21.1058862118175,-1.66783346591938));
#8966=CARTESIAN_POINT('Ctrl Pts',(-1.10271926064508,21.1089862646412,-1.67223640644865));
#8967=CARTESIAN_POINT('Ctrl Pts',(-1.09605031831596,21.1120789434068,-1.67659613043345));
#8968=CARTESIAN_POINT('Ctrl Pts',(-1.04927635614639,21.1337700650937,-1.70717392743191));
#8969=CARTESIAN_POINT('Ctrl Pts',(-1.00096181624318,21.1558248310677,-1.73596014723423));
#8970=CARTESIAN_POINT('Ctrl Pts',(-0.95132588988029,21.1781336136898,-1.76274783679009));
#8971=CARTESIAN_POINT('Ctrl Pts',(-0.901757245312855,21.2004121566235,-1.78949921547233));
#8972=CARTESIAN_POINT('Ctrl Pts',(-0.850871279746339,21.2229437755687,-1.814256943256));
#8973=CARTESIAN_POINT('Ctrl Pts',(-0.79892158787343,21.2456104589712,-1.83685197588009));
#8974=CARTESIAN_POINT('Ctrl Pts',(-0.746333987087704,21.2685554747151,-1.85972446101981));
#8975=CARTESIAN_POINT('Ctrl Pts',(-0.692656953597621,21.2916386061407,-1.88038028879146));
#8976=CARTESIAN_POINT('Ctrl Pts',(-0.638181784183411,21.314732447354,-1.89869031050386));
#8977=CARTESIAN_POINT('Ctrl Pts',(-0.584377988360444,21.3375416709098,-1.91677467224742));
#8978=CARTESIAN_POINT('Ctrl Pts',(-0.529796353858963,21.3603610388166,-1.93257054541442));
#8979=CARTESIAN_POINT('Ctrl Pts',(-0.474734811919399,21.383067410021,-1.94600301726812));
#8980=CARTESIAN_POINT('Ctrl Pts',(-0.418642668014323,21.406198782596,-1.95968690837756));
#8981=CARTESIAN_POINT('Ctrl Pts',(-0.362053244712395,21.4292125690608,-1.97091786454334));
#8982=CARTESIAN_POINT('Ctrl Pts',(-0.305288233051566,21.4519829129511,-1.97967168480661));
#8983=CARTESIAN_POINT('Ctrl Pts',(-0.248523221390737,21.4747532568414,-1.98842550506989));
#8984=CARTESIAN_POINT('Ctrl Pts',(-0.191583403285161,21.4972798769234,-1.99470232749285));
#8985=CARTESIAN_POINT('Ctrl Pts',(-0.134785361988912,21.5194457553878,-1.99853290967608));
#8986=CARTESIAN_POINT('Ctrl Pts',(-0.126823642526288,21.5225528784848,-1.9990698651771));
#8987=CARTESIAN_POINT('Ctrl Pts',(-0.118864689735969,21.5256529313082,-1.99955883944028));
#8988=CARTESIAN_POINT('Ctrl Pts',(-0.110909354270907,21.5287456100735,-2.));
#8989=CARTESIAN_POINT('Ctrl Pts',(-0.0551132738402241,21.5504366316392,
-2.00309415362571));
#8990=CARTESIAN_POINT('Ctrl Pts',(0.00112119338679578,21.572491294127,-2.00386648849132));
#8991=CARTESIAN_POINT('Ctrl Pts',(0.0575007497721895,21.59479997144,-2.00224737448708));
#8992=CARTESIAN_POINT('Ctrl Pts',(0.113804143497728,21.6170785121518,-2.00063044773009));
#8993=CARTESIAN_POINT('Ctrl Pts',(0.170251546614775,21.6396101294069,-1.99662830833388));
#8994=CARTESIAN_POINT('Ctrl Pts',(0.226538817573559,21.6622768116812,-1.9902213567835));
#8995=CARTESIAN_POINT('Ctrl Pts',(0.283517324818125,21.6852218523303,-1.98373572461284));
#8996=CARTESIAN_POINT('Ctrl Pts',(0.340330980853702,21.7083050095511,-1.97478568883787));
#8997=CARTESIAN_POINT('Ctrl Pts',(0.39666293982207,21.7313988770249,-1.96340505169883));
#8998=CARTESIAN_POINT('Ctrl Pts',(0.452300578005598,21.7542081005331,-1.95216468685026));
#8999=CARTESIAN_POINT('Ctrl Pts',(0.50746760100459,21.7770274688217,-1.9385535132094));
#9000=CARTESIAN_POINT('Ctrl Pts',(0.561868536374285,21.7997338408307,-1.92265561989074));
#9001=CARTESIAN_POINT('Ctrl Pts',(0.617287803076197,21.8228652535103,-1.90646013384186));
#9002=CARTESIAN_POINT('Ctrl Pts',(0.671911257217691,21.845879080117,-1.88789169564849));
#9003=CARTESIAN_POINT('Ctrl Pts',(0.725448204157765,21.868649463528,-1.86709019277301));
#9004=CARTESIAN_POINT('Ctrl Pts',(0.778985151097843,21.891419846939,-1.84628868989752));
#9005=CARTESIAN_POINT('Ctrl Pts',(0.83143498270472,21.9139465059182,-1.82325463286644));
#9006=CARTESIAN_POINT('Ctrl Pts',(0.882538907288783,21.9361124220507,-1.7981729510774));
#9007=CARTESIAN_POINT('Ctrl Pts',(0.889702436354614,21.939219545149,-1.79465710844931));
#9008=CARTESIAN_POINT('Ctrl Pts',(0.896839578792973,21.9423195979737,-1.79110109618647));
#9009=CARTESIAN_POINT('Ctrl Pts',(0.903949681684045,21.9454122767402,-1.78750548470437));
#9010=CARTESIAN_POINT('Ctrl Pts',(0.953817581608164,21.9671032983175,-1.76228706011861));
#9011=CARTESIAN_POINT('Ctrl Pts',(1.00290422625371,21.9891579608173,-1.73483868810305));
#9012=CARTESIAN_POINT('Ctrl Pts',(1.05092079735995,22.0114666381424,-1.70524671603297));
#9013=CARTESIAN_POINT('Ctrl Pts',(1.09887250325821,22.033745178851,-1.67569471952504));
#9014=CARTESIAN_POINT('Ctrl Pts',(1.14575631862848,22.0562767961026,-1.64400506358312));
#9015=CARTESIAN_POINT('Ctrl Pts',(1.19129904940493,22.0789434783733,-1.61031284530423));
#9016=CARTESIAN_POINT('Ctrl Pts',(1.23740106805828,22.1018885190206,-1.57620686946387));
#9017=CARTESIAN_POINT('Ctrl Pts',(1.28212811957486,22.1249716762396,-1.54004908310181));
#9018=CARTESIAN_POINT('Ctrl Pts',(1.32522270851242,22.1480655437115,-1.50202718274601));
#9019=CARTESIAN_POINT('Ctrl Pts',(1.36778613416513,22.1708747672221,-1.4644739221426));
#9020=CARTESIAN_POINT('Ctrl Pts',(1.40875659071607,22.1936941355131,-1.42510278848953));
#9021=CARTESIAN_POINT('Ctrl Pts',(1.44792023607921,22.2164005075243,-1.3841343413185));
#9022=CARTESIAN_POINT('Ctrl Pts',(1.4878169858694,22.2395319201999,-1.34239900562848));
#9023=CARTESIAN_POINT('Ctrl Pts',(1.52583806569387,22.2625457468024,-1.29900653938033));
#9024=CARTESIAN_POINT('Ctrl Pts',(1.56180167034017,22.2853161302094,-1.25422343599037));
#9025=CARTESIAN_POINT('Ctrl Pts',(1.59776527498648,22.3080865136163,-1.20944033260042));
#9026=CARTESIAN_POINT('Ctrl Pts',(1.63167113306028,22.3306131725915,-1.16326733826354));
#9027=CARTESIAN_POINT('Ctrl Pts',(1.66338758908297,22.3527790887203,-1.11599400238064));
#9028=CARTESIAN_POINT('Ctrl Pts',(1.6678334659193,22.3558862118176,-1.10936742881809));
#9029=CARTESIAN_POINT('Ctrl Pts',(1.6722364064486,22.3589862646413,-1.10271926064512));
#9030=CARTESIAN_POINT('Ctrl Pts',(1.67659613043341,22.3620789434069,-1.09605031831596));
#9031=CARTESIAN_POINT('Ctrl Pts',(1.70717378630092,22.383769964979,-1.04927657203033));
#9032=CARTESIAN_POINT('Ctrl Pts',(1.73595988153634,22.4058246274736,-1.00096226226136));
#9033=CARTESIAN_POINT('Ctrl Pts',(1.76274746587652,22.4281333047933,-0.951326577159854));
#9034=CARTESIAN_POINT('Ctrl Pts',(1.78949886308967,22.4504118455046,-0.901757944496487));
#9035=CARTESIAN_POINT('Ctrl Pts',(1.81425661025967,22.4729434627591,-0.850871989722196));
#9036=CARTESIAN_POINT('Ctrl Pts',(1.83685166293377,22.4956101450328,-0.798922307388034));
#9037=CARTESIAN_POINT('Ctrl Pts',(1.85972419433401,22.5185551856805,-0.746334656562013));
#9038=CARTESIAN_POINT('Ctrl Pts',(1.88038006400352,22.5416383428998,-0.692657569268785));
#9039=CARTESIAN_POINT('Ctrl Pts',(1.89869012261195,22.5647322103721,-0.638182343190864));
#9040=CARTESIAN_POINT('Ctrl Pts',(1.91677450019458,22.5875414338784,-0.584378552697299));
#9041=CARTESIAN_POINT('Ctrl Pts',(1.93257038954368,22.6103608021651,-0.52979692251304));
#9042=CARTESIAN_POINT('Ctrl Pts',(1.94600287774621,22.6330671741721,-0.474735383838417));
#9043=CARTESIAN_POINT('Ctrl Pts',(1.95968680875091,22.6561985868505,-0.418643147993864));
#9044=CARTESIAN_POINT('Ctrl Pts',(1.97091779663654,22.6792124134558,-0.362053629971188));
#9045=CARTESIAN_POINT('Ctrl Pts',(1.97967164017873,22.7019827968656,-0.305288522445268));
#9046=CARTESIAN_POINT('Ctrl Pts',(1.98842548372092,22.7247531802754,-0.248523414919351));
#9047=CARTESIAN_POINT('Ctrl Pts',(1.99470232098272,22.7472798392533,-0.191583499811085));
#9048=CARTESIAN_POINT('Ctrl Pts',(1.99853290967555,22.7694457553847,-0.134785361996723));
#9049=CARTESIAN_POINT('Ctrl Pts',(1.99906986517678,22.7725528784828,-0.126823642531481));
#9050=CARTESIAN_POINT('Ctrl Pts',(1.99955883944014,22.7756529313072,-0.118864689738578));
#9051=CARTESIAN_POINT('Ctrl Pts',(2.,22.7787456100735,-0.110909354270901));
#9052=CARTESIAN_POINT('Ctrl Pts',(2.00309415362582,22.8004366316399,-0.0551132738382789));
#9053=CARTESIAN_POINT('Ctrl Pts',(2.00386648849139,22.8224912941286,0.00112119339068031));
#9054=CARTESIAN_POINT('Ctrl Pts',(2.00224737448693,22.8447999714423,0.0575007497779818));
#9055=CARTESIAN_POINT('Ctrl Pts',(2.00063044773006,22.8670785121501,0.11380414349335));
#9056=CARTESIAN_POINT('Ctrl Pts',(1.99662830833485,22.8896101294011,0.17025154660023));
#9057=CARTESIAN_POINT('Ctrl Pts',(1.99022135678632,22.9122768116713,0.226538817548881));
#9058=CARTESIAN_POINT('Ctrl Pts',(1.98373572461611,22.9352218523213,0.283517324795811));
#9059=CARTESIAN_POINT('Ctrl Pts',(1.97478568884138,22.958305009543,0.340330980833825));
#9060=CARTESIAN_POINT('Ctrl Pts',(1.96340505170238,22.9813988770177,0.396662939804617));
#9061=CARTESIAN_POINT('Ctrl Pts',(1.95216468685371,23.0042081005271,0.452300577991144));
#9062=CARTESIAN_POINT('Ctrl Pts',(1.93855351321251,23.027027468817,0.507467600993079));
#9063=CARTESIAN_POINT('Ctrl Pts',(1.92265561989324,23.0497338408271,0.561868536365727));
#9064=CARTESIAN_POINT('Ctrl Pts',(1.90646013384401,23.0728652535076,0.617287803069753));
#9065=CARTESIAN_POINT('Ctrl Pts',(1.88789169565015,23.0958790801151,0.671911257213199));
#9066=CARTESIAN_POINT('Ctrl Pts',(1.86709019277399,23.1186494635269,0.725448204155213));
#9067=CARTESIAN_POINT('Ctrl Pts',(1.84628868989783,23.1414198469387,0.778985151097228));
#9068=CARTESIAN_POINT('Ctrl Pts',(1.82325463286591,23.1639465059187,0.831434982705977));
#9069=CARTESIAN_POINT('Ctrl Pts',(1.79817295107589,23.1861124220521,0.88253890729181));
#9070=CARTESIAN_POINT('Ctrl Pts',(1.79465710844828,23.1892195451499,0.88970243635662));
#9071=CARTESIAN_POINT('Ctrl Pts',(1.79110109618594,23.1923195979741,0.896839578793966));
#9072=CARTESIAN_POINT('Ctrl Pts',(1.78750548470435,23.1954122767402,0.903949681684032));
#9073=CARTESIAN_POINT('Ctrl Pts',(1.76228706012777,23.2171032983096,0.953817581590012));
#9074=CARTESIAN_POINT('Ctrl Pts',(1.73483868812302,23.2391579608013,1.00290422621798));
#9075=CARTESIAN_POINT('Ctrl Pts',(1.70524671606526,23.2614666381181,1.05092079730752));
#9076=CARTESIAN_POINT('Ctrl Pts',(1.6756947195636,23.2837451788229,1.09887250319891));
#9077=CARTESIAN_POINT('Ctrl Pts',(1.64400506362857,23.3062767960707,1.14575631856278));
#9078=CARTESIAN_POINT('Ctrl Pts',(1.61031284535712,23.3289434783377,1.19129904933341));
#9079=CARTESIAN_POINT('Ctrl Pts',(1.57620686951458,23.3518885189878,1.23740106799398));
#9080=CARTESIAN_POINT('Ctrl Pts',(1.54004908314973,23.3749716762096,1.28212811951758));
#9081=CARTESIAN_POINT('Ctrl Pts',(1.5020271827906,23.3980655436844,1.32522270846184));
#9082=CARTESIAN_POINT('Ctrl Pts',(1.46447392219389,23.4208747671917,1.36778613410986));
#9083=CARTESIAN_POINT('Ctrl Pts',(1.42510278854796,23.4436941354796,1.40875659065662));
#9084=CARTESIAN_POINT('Ctrl Pts',(1.38413434138436,23.4664005074878,1.44792023601622));
#9085=CARTESIAN_POINT('Ctrl Pts',(1.34239900568539,23.4895319201694,1.48781698581861));
#9086=CARTESIAN_POINT('Ctrl Pts',(1.29900653942732,23.5125457467779,1.52583806565439));
#9087=CARTESIAN_POINT('Ctrl Pts',(1.25422343602664,23.5353161301909,1.56180167031102));
#9088=CARTESIAN_POINT('Ctrl Pts',(1.20944033262596,23.5580865136038,1.59776527496766));
#9089=CARTESIAN_POINT('Ctrl Pts',(1.1632673382776,23.5806131725848,1.63167113305074));
#9090=CARTESIAN_POINT('Ctrl Pts',(1.11599400238262,23.6027790887192,1.66338758908162));
#9091=CARTESIAN_POINT('Ctrl Pts',(1.10936742881941,23.6058862118168,1.6678334659184));
#9092=CARTESIAN_POINT('Ctrl Pts',(1.10271926064578,23.6089862646409,1.67223640644814));
#9093=CARTESIAN_POINT('Ctrl Pts',(1.09605031831596,23.6120789434068,1.67659613043339));
#9094=CARTESIAN_POINT('Ctrl Pts',(1.0492765720368,23.6337699649759,1.70717378629669));
#9095=CARTESIAN_POINT('Ctrl Pts',(1.00096226227484,23.6558246274673,1.73595988152832));
#9096=CARTESIAN_POINT('Ctrl Pts',(0.951326577180585,23.6781333047839,1.76274746586534));
#9097=CARTESIAN_POINT('Ctrl Pts',(0.901757944510291,23.7004118454984,1.78949886308298));
#9098=CARTESIAN_POINT('Ctrl Pts',(0.850871989728759,23.7229434627562,1.81425661025687));
#9099=CARTESIAN_POINT('Ctrl Pts',(0.798922307386955,23.7456101450332,1.83685166293425));
#9100=CARTESIAN_POINT('Ctrl Pts',(0.746334656561049,23.7685551856808,1.8597241943344));
#9101=CARTESIAN_POINT('Ctrl Pts',(0.692657569267959,23.7916383429002,1.88038006400383));
#9102=CARTESIAN_POINT('Ctrl Pts',(0.638182343190171,23.8147322103724,1.89869012261219));
#9103=CARTESIAN_POINT('Ctrl Pts',(0.584378552694931,23.8375414338794,1.91677450019536));
#9104=CARTESIAN_POINT('Ctrl Pts',(0.529796922509002,23.8603608021668,1.93257038954484));
#9105=CARTESIAN_POINT('Ctrl Pts',(0.474735383832642,23.8830671741745,1.94600287774763));
#9106=CARTESIAN_POINT('Ctrl Pts',(0.418643147989125,23.9061985868524,1.95968680875189));
#9107=CARTESIAN_POINT('Ctrl Pts',(0.362053629967556,23.9292124134573,1.97091779663716));
#9108=CARTESIAN_POINT('Ctrl Pts',(0.305288522442711,23.9519827968666,1.97967164017911));
#9109=CARTESIAN_POINT('Ctrl Pts',(0.248523414917863,23.974753180276,1.98842548372106));
#9110=CARTESIAN_POINT('Ctrl Pts',(0.191583499810712,23.9972798392535,1.9947023209827));
#9111=CARTESIAN_POINT('Ctrl Pts',(0.13478536199745,24.0194457553844,1.99853290967547));
#9112=CARTESIAN_POINT('Ctrl Pts',(0.126823642531985,24.0225528784826,1.99906986517672));
#9113=CARTESIAN_POINT('Ctrl Pts',(0.118864689738828,24.0256529313071,1.9995588394401));
#9114=CARTESIAN_POINT('Ctrl Pts',(0.110909354270918,24.0287456100735,1.99999999999998));
#9115=CARTESIAN_POINT('Ctrl Pts',(0.0551130162975314,24.0504367317603,2.00309416790767));
#9116=CARTESIAN_POINT('Ctrl Pts',(-0.00112171253166826,24.0724914977342,
2.00386649558389));
#9117=CARTESIAN_POINT('Ctrl Pts',(-0.0575015304798811,24.0948002803561,
2.00224735206656));
#9118=CARTESIAN_POINT('Ctrl Pts',(-0.113805823015011,24.1170791785251,2.00063037752543));
#9119=CARTESIAN_POINT('Ctrl Pts',(-0.170254128158742,24.1396111607935,1.99662811395759));
#9120=CARTESIAN_POINT('Ctrl Pts',(-0.2265422897397,24.1622782099103,1.99022096155788));
#9121=CARTESIAN_POINT('Ctrl Pts',(-0.283520500950918,24.1852231396404,1.98373526239061));
#9122=CARTESIAN_POINT('Ctrl Pts',(-0.340333856155103,24.2083061819791,1.97478518482606));
#9123=CARTESIAN_POINT('Ctrl Pts',(-0.396665514397027,24.2313999324986,1.96340453156067));
#9124=CARTESIAN_POINT('Ctrl Pts',(-0.452303137861108,24.2542091562259,1.95216409375152));
#9125=CARTESIAN_POINT('Ctrl Pts',(-0.507470141472793,24.2770285228212,1.93855284808134));
#9126=CARTESIAN_POINT('Ctrl Pts',(-0.561871053025202,24.2997348912542,1.92265488443379));
#9127=CARTESIAN_POINT('Ctrl Pts',(-0.61728987625894,24.3228661253192,1.90645944924681));
#9128=CARTESIAN_POINT('Ctrl Pts',(-0.671912894410742,24.3458797731456,1.88789109964264));
#9129=CARTESIAN_POINT('Ctrl Pts',(-0.725449419744559,24.3686499805425,1.86708972046256));
#9130=CARTESIAN_POINT('Ctrl Pts',(-0.778985945078376,24.3914201879394,1.84628834128247));
#9131=CARTESIAN_POINT('Ctrl Pts',(-0.831435369486437,24.4139466736816,1.82325444303487));
#9132=CARTESIAN_POINT('Ctrl Pts',(-0.882538907289412,24.436112422051,1.79817295107701));
#9133=CARTESIAN_POINT('Ctrl Pts',(-0.889702436355033,24.4392195451492,1.79465710844901));
#9134=CARTESIAN_POINT('Ctrl Pts',(-0.896839578793186,24.4423195979737,1.79110109618628));
#9135=CARTESIAN_POINT('Ctrl Pts',(-0.903949681684042,24.4454122767402,1.78750548470429));
#9136=CARTESIAN_POINT('Ctrl Pts',(-0.953817581595852,24.4671032983121,1.76228706012477));
#9137=CARTESIAN_POINT('Ctrl Pts',(-1.00290422622947,24.4891579608064,1.73483868811654));
#9138=CARTESIAN_POINT('Ctrl Pts',(-1.05092079732441,24.5114666381259,1.7052467160548));
#9139=CARTESIAN_POINT('Ctrl Pts',(-1.09887250319947,24.5337451788233,1.67569471956254));
#9140=CARTESIAN_POINT('Ctrl Pts',(-1.14575631854775,24.5562767960636,1.64400506363834));
#9141=CARTESIAN_POINT('Ctrl Pts',(-1.19129904930367,24.578943478323,1.61031284537906));
#9142=CARTESIAN_POINT('Ctrl Pts',(-1.23740106796711,24.6018885189741,1.57620686953571));
#9143=CARTESIAN_POINT('Ctrl Pts',(-1.28212811949352,24.6249716761971,1.54004908316981));
#9144=CARTESIAN_POINT('Ctrl Pts',(-1.32522270844045,24.648065543673,1.50202718280942));
#9145=CARTESIAN_POINT('Ctrl Pts',(-1.36778613409947,24.6708747671859,1.46447392220408));
#9146=CARTESIAN_POINT('Ctrl Pts',(-1.4087565906565,24.6936941354794,1.42510278854858));
#9147=CARTESIAN_POINT('Ctrl Pts',(-1.44792023602544,24.7164005074931,1.38413434137467));
#9148=CARTESIAN_POINT('Ctrl Pts',(-1.48781698582565,24.7395319201737,1.34239900567742));
#9149=CARTESIAN_POINT('Ctrl Pts',(-1.52583806565949,24.7625457467811,1.29900653942118));
#9150=CARTESIAN_POINT('Ctrl Pts',(-1.56180167031431,24.7853161301929,1.25422343602251));
#9151=CARTESIAN_POINT('Ctrl Pts',(-1.59776527496913,24.8080865136048,1.20944033262385));
#9152=CARTESIAN_POINT('Ctrl Pts',(-1.63167113305059,24.8306131725848,1.16326733827763));
#9153=CARTESIAN_POINT('Ctrl Pts',(-1.66338758908004,24.8527790887181,1.11599400238492));
#9154=CARTESIAN_POINT('Ctrl Pts',(-1.66783346591736,24.8558862118161,1.10936742882094));
#9155=CARTESIAN_POINT('Ctrl Pts',(-1.67223640644764,24.8589862646405,1.10271926064652));
#9156=CARTESIAN_POINT('Ctrl Pts',(-1.6765961304334,24.8620789434068,1.09605031831592));
#9157=CARTESIAN_POINT('Ctrl Pts',(-1.7071737863027,24.8837699649802,1.04927657202758));
#9158=CARTESIAN_POINT('Ctrl Pts',(-1.73595988153965,24.905824627476,1.00096226225577));
#9159=CARTESIAN_POINT('Ctrl Pts',(-1.76274746588115,24.9281333047971,0.951326577151247));
#9160=CARTESIAN_POINT('Ctrl Pts',(-1.78949886308653,24.9504118455021,0.901757944501721));
#9161=CARTESIAN_POINT('Ctrl Pts',(-1.81425661024985,24.9729434627502,0.850871989742079));
#9162=CARTESIAN_POINT('Ctrl Pts',(-1.83685166291854,24.9956101450174,0.798922307423065));
#9163=CARTESIAN_POINT('Ctrl Pts',(-1.85972419432098,25.0185551856663,0.746334656594723));
#9164=CARTESIAN_POINT('Ctrl Pts',(-1.88038006399248,25.0416383428869,0.692657569299052));
#9165=CARTESIAN_POINT('Ctrl Pts',(-1.89869012260265,25.0647322103604,0.638182343218542));
#9166=CARTESIAN_POINT('Ctrl Pts',(-1.91677450018681,25.0875414338675,0.584378552723056));
#9167=CARTESIAN_POINT('Ctrl Pts',(-1.93257038953726,25.1103608021552,0.529796922536758));
#9168=CARTESIAN_POINT('Ctrl Pts',(-1.94600287774096,25.1330671741632,0.474735383859972));
#9169=CARTESIAN_POINT('Ctrl Pts',(-1.95968680874709,25.156198586843,0.418643148012222));
#9170=CARTESIAN_POINT('Ctrl Pts',(-1.97091779663386,25.1792124134497,0.362053629986285));
#9171=CARTESIAN_POINT('Ctrl Pts',(-1.97967164017691,25.2019827968609,0.305288522457018));
#9172=CARTESIAN_POINT('Ctrl Pts',(-1.98842548371996,25.224753180272,0.248523414927751));
#9173=CARTESIAN_POINT('Ctrl Pts',(-1.99470232098232,25.2472798392513,0.191583499816204));
#9174=CARTESIAN_POINT('Ctrl Pts',(-1.99853290967542,25.269445755384,0.134785361998493));
#9175=CARTESIAN_POINT('Ctrl Pts',(-1.9990698651767,25.2725528784823,0.126823642532641));
#9176=CARTESIAN_POINT('Ctrl Pts',(-1.9995588394401,25.2756529313069,0.118864689739151));
#9177=CARTESIAN_POINT('Ctrl Pts',(-2.,25.2787456100735,0.110909354270877));
#9178=CARTESIAN_POINT('Ctrl Pts',(-2.00309415362697,25.300436631648,0.0551132738174295));
#9179=CARTESIAN_POINT('Ctrl Pts',(-2.00386648849195,25.322491294145,-0.00112119343270661));
#9180=CARTESIAN_POINT('Ctrl Pts',(-2.00224737448511,25.3447999714672,-0.0575007498411724));
#9181=CARTESIAN_POINT('Ctrl Pts',(-2.00063044772582,25.367078512184,-0.113804143578793));
#9182=CARTESIAN_POINT('Ctrl Pts',(-1.9966283083263,25.3896101294441,-0.170251546707902));
#9183=CARTESIAN_POINT('Ctrl Pts',(-1.99022135677158,25.4122768117234,-0.22653881767843));
#9184=CARTESIAN_POINT('Ctrl Pts',(-1.98373572459887,25.4352218523693,-0.283517324914314));
#9185=CARTESIAN_POINT('Ctrl Pts',(-1.97478568882256,25.4583050095867,-0.34033098094112));
#9186=CARTESIAN_POINT('Ctrl Pts',(-1.96340505168295,25.4813988770571,-0.396662939900708));
#9187=CARTESIAN_POINT('Ctrl Pts',(-1.95216468683355,25.5042081005624,-0.452300578076878));
#9188=CARTESIAN_POINT('Ctrl Pts',(-1.93855351319249,25.5270274688482,-0.50746760106841));
#9189=CARTESIAN_POINT('Ctrl Pts',(-1.92265561987421,25.5497338408542,-0.561868536430838));
#9190=CARTESIAN_POINT('Ctrl Pts',(-1.9064601338263,25.5728652535301,-0.617287803123396));
#9191=CARTESIAN_POINT('Ctrl Pts',(-1.8878916956347,25.5958790801329,-0.671911257255631));
#9192=CARTESIAN_POINT('Ctrl Pts',(-1.86709019276172,25.6186494635402,-0.725448204186784));
#9193=CARTESIAN_POINT('Ctrl Pts',(-1.84628868988873,25.6414198469475,-0.77898515111794));
#9194=CARTESIAN_POINT('Ctrl Pts',(-1.82325463286093,25.663946505923,-0.831434982716144));
#9195=CARTESIAN_POINT('Ctrl Pts',(-1.79817295107583,25.686112422052,-0.882538907291945));
#9196=CARTESIAN_POINT('Ctrl Pts',(-1.79465710844823,25.6892195451498,-0.889702436356714));
#9197=CARTESIAN_POINT('Ctrl Pts',(-1.79110109618591,25.692319597974,-0.896839578794057));
#9198=CARTESIAN_POINT('Ctrl Pts',(-1.78750548470433,25.6954122767401,-0.903949681684092));
#9199=CARTESIAN_POINT('Ctrl Pts',(-1.7622870601227,25.7171032983138,-0.953817581600028));
#9200=CARTESIAN_POINT('Ctrl Pts',(-1.73483868811199,25.7391579608101,-1.00290422623769));
#9201=CARTESIAN_POINT('Ctrl Pts',(-1.70524671604744,25.7614666381315,-1.05092079733642));
#9202=CARTESIAN_POINT('Ctrl Pts',(-1.67569471954384,25.7837451788372,-1.09887250322914));
#9203=CARTESIAN_POINT('Ctrl Pts',(-1.64400506360674,25.806276796086,-1.14575631859421));
#9204=CARTESIAN_POINT('Ctrl Pts',(-1.61031284533311,25.8289434783539,-1.19129904936587));
#9205=CARTESIAN_POINT('Ctrl Pts',(-1.57620686949147,25.8518885190027,-1.23740106802327));
#9206=CARTESIAN_POINT('Ctrl Pts',(-1.54004908312781,25.8749716762233,-1.28212811954378));
#9207=CARTESIAN_POINT('Ctrl Pts',(-1.5020271827701,25.8980655436969,-1.3252227084851));
#9208=CARTESIAN_POINT('Ctrl Pts',(-1.46447392217107,25.9208747672052,-1.36778613413441));
#9209=CARTESIAN_POINT('Ctrl Pts',(-1.42510278852273,25.943694135494,-1.40875659068227));
#9210=CARTESIAN_POINT('Ctrl Pts',(-1.38413434135664,25.9664005075031,-1.44792023604275));
#9211=CARTESIAN_POINT('Ctrl Pts',(-1.34239900566126,25.9895319201823,-1.48781698584017));
#9212=CARTESIAN_POINT('Ctrl Pts',(-1.29900653940712,26.0125457467884,-1.52583806567139));
#9213=CARTESIAN_POINT('Ctrl Pts',(-1.25422343601075,26.035316130199,-1.56180167032382));
#9214=CARTESIAN_POINT('Ctrl Pts',(-1.20944033261438,26.0580865136095,-1.59776527497625));
#9215=CARTESIAN_POINT('Ctrl Pts',(-1.16326733827057,26.0806131725882,-1.63167113305559));
#9216=CARTESIAN_POINT('Ctrl Pts',(-1.11599400238044,26.1027790887203,-1.66338758908314));
#9217=CARTESIAN_POINT('Ctrl Pts',(-1.10936742881793,26.1058862118175,-1.66783346591944));
#9218=CARTESIAN_POINT('Ctrl Pts',(-1.10271926064503,26.1089862646412,-1.67223640644869));
#9219=CARTESIAN_POINT('Ctrl Pts',(-1.09605031831595,26.1120789434068,-1.67659613043346));
#9220=CARTESIAN_POINT('Ctrl Pts',(-1.04927657203578,26.1337699649764,-1.7071737862974));
#9221=CARTESIAN_POINT('Ctrl Pts',(-1.00096226227268,26.1558246274683,-1.73595988152965));
#9222=CARTESIAN_POINT('Ctrl Pts',(-0.951326577177282,26.1781333047854,-1.76274746586717));
#9223=CARTESIAN_POINT('Ctrl Pts',(-0.901757944517214,26.2004118454953,-1.78949886307917));
#9224=CARTESIAN_POINT('Ctrl Pts',(-0.850871989746337,26.2229434627484,-1.8142566102483));
#9225=CARTESIAN_POINT('Ctrl Pts',(-0.798922307415678,26.2456101450206,-1.8368516629218));
#9226=CARTESIAN_POINT('Ctrl Pts',(-0.74633465658777,26.2685551856693,-1.8597241943238));
#9227=CARTESIAN_POINT('Ctrl Pts',(-0.692657569292552,26.2916383428896,-1.8803800639949));
#9228=CARTESIAN_POINT('Ctrl Pts',(-0.638182343212506,26.3147322103629,-1.89869012260473));
#9229=CARTESIAN_POINT('Ctrl Pts',(-0.584378552725403,26.3375414338665,-1.91677450018587));
#9230=CARTESIAN_POINT('Ctrl Pts',(-0.529796922547766,26.3603608021506,-1.93257038953402));
#9231=CARTESIAN_POINT('Ctrl Pts',(-0.474735383879798,26.383067174155,-1.94600287773618));
#9232=CARTESIAN_POINT('Ctrl Pts',(-0.418643148028719,26.4061985868363,-1.95968680874373));
#9233=CARTESIAN_POINT('Ctrl Pts',(-0.362053629999354,26.4292124134444,-1.97091779663162));
#9234=CARTESIAN_POINT('Ctrl Pts',(-0.305288522466675,26.451982796857,-1.97967164017548));
#9235=CARTESIAN_POINT('Ctrl Pts',(-0.248523414933991,26.4747531802696,-1.98842548371934));
#9236=CARTESIAN_POINT('Ctrl Pts',(-0.191583499818795,26.4972798392503,-1.99470232098221));
#9237=CARTESIAN_POINT('Ctrl Pts',(-0.13478536199757,26.5194457553844,-1.99853290967552));
#9238=CARTESIAN_POINT('Ctrl Pts',(-0.126823642532062,26.5225528784825,-1.99906986517677));
#9239=CARTESIAN_POINT('Ctrl Pts',(-0.118864689738849,26.5256529313071,-1.99955883944015));
#9240=CARTESIAN_POINT('Ctrl Pts',(-0.110909354270907,26.5287456100735,-2.00000000000003));
#9241=CARTESIAN_POINT('Ctrl Pts',(-0.0551132738153703,26.5504366316488,
-2.00309415362711));
#9242=CARTESIAN_POINT('Ctrl Pts',(0.00112119343692078,26.5724912941467,
-2.00386648849203));
#9243=CARTESIAN_POINT('Ctrl Pts',(0.0575007498475077,26.5947999714698,-2.00224737448494));
#9244=CARTESIAN_POINT('Ctrl Pts',(0.113804143574996,26.6170785121825,-2.00063044772577));
#9245=CARTESIAN_POINT('Ctrl Pts',(0.170251546693887,26.6396101294386,-1.99662830832721));
#9246=CARTESIAN_POINT('Ctrl Pts',(0.22653881765432,26.6622768117137,-1.99022135677433));
#9247=CARTESIAN_POINT('Ctrl Pts',(0.283517324892532,26.6852218523605,-1.98373572460205));
#9248=CARTESIAN_POINT('Ctrl Pts',(0.3403309809217,26.7083050095789,-1.97478568882598));
#9249=CARTESIAN_POINT('Ctrl Pts',(0.396662939883625,26.7313988770501,-1.96340505168641));
#9250=CARTESIAN_POINT('Ctrl Pts',(0.452300578058839,26.754208100555,-1.9521646868377));
#9251=CARTESIAN_POINT('Ctrl Pts',(0.507467601049452,26.7770274688404,-1.93855351319744));
#9252=CARTESIAN_POINT('Ctrl Pts',(0.561868536411038,26.799733840846,-1.92265561988001));
#9253=CARTESIAN_POINT('Ctrl Pts',(0.617287803107586,26.8228652535235,-1.90646013383155));
#9254=CARTESIAN_POINT('Ctrl Pts',(0.671911257243766,26.845879080128,-1.88789169563905));
#9255=CARTESIAN_POINT('Ctrl Pts',(0.725448204178672,26.8686494635369,-1.86709019276489));
#9256=CARTESIAN_POINT('Ctrl Pts',(0.778985151113583,26.8914198469457,-1.84628868989072));
#9257=CARTESIAN_POINT('Ctrl Pts',(0.831434982715474,26.9139465059228,-1.82325463286138));
#9258=CARTESIAN_POINT('Ctrl Pts',(0.882538907294795,26.9361124220533,-1.79817295107445));
#9259=CARTESIAN_POINT('Ctrl Pts',(0.889702436358604,26.9392195451507,-1.79465710844732));
#9260=CARTESIAN_POINT('Ctrl Pts',(0.896839578794966,26.9423195979745,-1.79110109618546));
#9261=CARTESIAN_POINT('Ctrl Pts',(0.903949681684054,26.9454122767402,-1.78750548470436));
#9262=CARTESIAN_POINT('Ctrl Pts',(0.953817581590833,26.9671032983099,-1.76228706012734));
#9263=CARTESIAN_POINT('Ctrl Pts',(1.0029042262196,26.989157960802,-1.73483868812211));
#9264=CARTESIAN_POINT('Ctrl Pts',(1.05092079730992,27.0114666381192,-1.70524671606377));
#9265=CARTESIAN_POINT('Ctrl Pts',(1.09887250322323,27.0337451788342,-1.67569471954849));
#9266=CARTESIAN_POINT('Ctrl Pts',(1.14575631860802,27.0562767960925,-1.64400506359792));
#9267=CARTESIAN_POINT('Ctrl Pts',(1.19129904939823,27.07894347837,-1.61031284530915));
#9268=CARTESIAN_POINT('Ctrl Pts',(1.23740106805221,27.1018885190175,-1.5762068694686));
#9269=CARTESIAN_POINT('Ctrl Pts',(1.28212811956941,27.1249716762368,-1.54004908310631));
#9270=CARTESIAN_POINT('Ctrl Pts',(1.32522270850755,27.1480655437089,-1.50202718275025));
#9271=CARTESIAN_POINT('Ctrl Pts',(1.36778613415706,27.1708747672177,-1.46447392214992));
#9272=CARTESIAN_POINT('Ctrl Pts',(1.40875659070502,27.1936941355069,-1.42510278850023));
#9273=CARTESIAN_POINT('Ctrl Pts',(1.44792023606551,27.2164005075163,-1.38413434133279));
#9274=CARTESIAN_POINT('Ctrl Pts',(1.48781698585827,27.2395319201932,-1.34239900564092));
#9275=CARTESIAN_POINT('Ctrl Pts',(1.52583806568516,27.262545746797,-1.29900653939066));
#9276=CARTESIAN_POINT('Ctrl Pts',(1.56180167033367,27.2853161302052,-1.25422343599845));
#9277=CARTESIAN_POINT('Ctrl Pts',(1.59776527498217,27.3080865136134,-1.20944033260624));
#9278=CARTESIAN_POINT('Ctrl Pts',(1.63167113305793,27.3306131725898,-1.16326733826698));
#9279=CARTESIAN_POINT('Ctrl Pts',(1.66338758908235,27.3527790887197,-1.11599400238156));
#9280=CARTESIAN_POINT('Ctrl Pts',(1.6678334659189,27.3558862118172,-1.1093674288187));
#9281=CARTESIAN_POINT('Ctrl Pts',(1.6722364064484,27.3589862646411,-1.10271926064542));
#9282=CARTESIAN_POINT('Ctrl Pts',(1.67659613043341,27.3620789434068,-1.09605031831596));
#9283=CARTESIAN_POINT('Ctrl Pts',(1.70717378629165,27.3837699649724,-1.04927657204452));
#9284=CARTESIAN_POINT('Ctrl Pts',(1.73595988151885,27.4058246274601,-1.00096226229075));
#9285=CARTESIAN_POINT('Ctrl Pts',(1.76274746585211,27.4281333047729,-0.951326577205113));
#9286=CARTESIAN_POINT('Ctrl Pts',(1.78949886307212,27.4504118454887,-0.901757944532073));
#9287=CARTESIAN_POINT('Ctrl Pts',(1.81425661024819,27.472943462748,-0.850871989747507));
#9288=CARTESIAN_POINT('Ctrl Pts',(1.83685166292746,27.4956101450264,-0.798922307402572));
#9289=CARTESIAN_POINT('Ctrl Pts',(1.85972419432879,27.5185551856747,-0.746334656575189));
#9290=CARTESIAN_POINT('Ctrl Pts',(1.88038006399926,27.5416383428948,-0.692657569280544));
#9291=CARTESIAN_POINT('Ctrl Pts',(1.8986901226085,27.5647322103678,-0.638182343201152));
#9292=CARTESIAN_POINT('Ctrl Pts',(1.91677450019326,27.5875414338763,-0.58437855270225));
#9293=CARTESIAN_POINT('Ctrl Pts',(1.93257038954402,27.6103608021654,-0.529796922512431));
#9294=CARTESIAN_POINT('Ctrl Pts',(1.94600287774773,27.6330671741746,-0.474735383832203));
#9295=CARTESIAN_POINT('Ctrl Pts',(1.95968680875216,27.6561985868529,-0.418643147987978));
#9296=CARTESIAN_POINT('Ctrl Pts',(1.97091779663755,27.6792124134581,-0.362053629965651));
#9297=CARTESIAN_POINT('Ctrl Pts',(1.97967164017953,27.7019827968677,-0.305288522440102));
#9298=CARTESIAN_POINT('Ctrl Pts',(1.98842548372151,27.7247531802773,-0.248523414914553));
#9299=CARTESIAN_POINT('Ctrl Pts',(1.99470232098313,27.7472798392551,-0.191583499806667));
#9300=CARTESIAN_POINT('Ctrl Pts',(1.99853290967581,27.7694457553863,-0.13478536199265));
#9301=CARTESIAN_POINT('Ctrl Pts',(1.99906986517693,27.7725528784838,-0.126823642528799));
#9302=CARTESIAN_POINT('Ctrl Pts',(1.9995588394402,27.7756529313077,-0.118864689737254));
#9303=CARTESIAN_POINT('Ctrl Pts',(1.99999999999999,27.7787456100735,-0.110909354270966));
#9304=CARTESIAN_POINT('Ctrl Pts',(2.00309415362701,27.8004366316483,-0.0551132738167583));
#9305=CARTESIAN_POINT('Ctrl Pts',(2.00386648849197,27.8224912941456,0.00112119343414613));
#9306=CARTESIAN_POINT('Ctrl Pts',(2.00224737448504,27.8447999714681,0.0575007498433761));
#9307=CARTESIAN_POINT('Ctrl Pts',(2.00063044772619,27.8670785121781,0.113804143563829));
#9308=CARTESIAN_POINT('Ctrl Pts',(1.99662830832856,27.8896101294313,0.170251546675671));
#9309=CARTESIAN_POINT('Ctrl Pts',(1.99022135677719,27.9122768117036,0.226538817629131));
#9310=CARTESIAN_POINT('Ctrl Pts',(1.98373572460543,27.935221852351,0.283517324869203));
#9311=CARTESIAN_POINT('Ctrl Pts',(1.97478568882973,27.9583050095701,0.340330980900261));
#9312=CARTESIAN_POINT('Ctrl Pts',(1.96340505169036,27.9813988770421,0.396662939864062));
#9313=CARTESIAN_POINT('Ctrl Pts',(1.95216468683788,28.0042081005558,0.452300578060788));
#9314=CARTESIAN_POINT('Ctrl Pts',(1.93855351319197,28.02702746885,0.507467601072668));
#9315=CARTESIAN_POINT('Ctrl Pts',(1.9226556198672,28.0497338408643,0.561868536454782));
#9316=CARTESIAN_POINT('Ctrl Pts',(1.9064601338198,28.0728652535385,0.617287803143049));
#9317=CARTESIAN_POINT('Ctrl Pts',(1.88789169562905,28.0958790801396,0.671911257271115));
#9318=CARTESIAN_POINT('Ctrl Pts',(1.86709019275729,28.1186494635452,0.725448204198153));
#9319=CARTESIAN_POINT('Ctrl Pts',(1.84628868988553,28.1414198469507,0.778985151125196));
#9320=CARTESIAN_POINT('Ctrl Pts',(1.82325463285926,28.1639465059246,0.831434982719507));
#9321=CARTESIAN_POINT('Ctrl Pts',(1.79817295107597,28.186112422052,0.882538907291619));
#9322=CARTESIAN_POINT('Ctrl Pts',(1.79465710844833,28.1892195451498,0.889702436356488));
#9323=CARTESIAN_POINT('Ctrl Pts',(1.79110109618595,28.1923195979741,0.896839578793933));
#9324=CARTESIAN_POINT('Ctrl Pts',(1.78750548470432,28.1954122767402,0.903949681684058));
#9325=CARTESIAN_POINT('Ctrl Pts',(1.76228706011533,28.2171032983203,0.953817581614572));
#9326=CARTESIAN_POINT('Ctrl Pts',(1.73483868809596,28.239157960823,1.00290422626632));
#9327=CARTESIAN_POINT('Ctrl Pts',(1.70524671602152,28.2614666381511,1.05092079737846));
#9328=CARTESIAN_POINT('Ctrl Pts',(1.67569471951602,28.2837451788574,1.0988725032716));
#9329=CARTESIAN_POINT('Ctrl Pts',(1.64400506357697,28.3062767961068,1.14575631863696));
#9330=CARTESIAN_POINT('Ctrl Pts',(1.61031284530134,28.3289434783753,1.19129904940878));
#9331=CARTESIAN_POINT('Ctrl Pts',(1.57620686946125,28.3518885190223,1.23740106806151));
#9332=CARTESIAN_POINT('Ctrl Pts',(1.54004908309952,28.3749716762411,1.2821281195775));
#9333=CARTESIAN_POINT('Ctrl Pts',(1.50202718274414,28.3980655437126,1.32522270851447));
#9334=CARTESIAN_POINT('Ctrl Pts',(1.46447392213801,28.4208747672248,1.36778613417015));
#9335=CARTESIAN_POINT('Ctrl Pts',(1.42510278848197,28.4436941355174,1.40875659072383));
#9336=CARTESIAN_POINT('Ctrl Pts',(1.38413434130772,28.4664005075303,1.44792023608946));
#9337=CARTESIAN_POINT('Ctrl Pts',(1.34239900561962,28.4895319202046,1.48781698587723));
#9338=CARTESIAN_POINT('Ctrl Pts',(1.29900653937359,28.5125457468058,1.52583806569944));
#9339=CARTESIAN_POINT('Ctrl Pts',(1.25422343598591,28.5353161302116,1.56180167034371));
#9340=CARTESIAN_POINT('Ctrl Pts',(1.20944033259823,28.5580865136173,1.59776527498798));
#9341=CARTESIAN_POINT('Ctrl Pts',(1.16326733826385,28.5806131725913,1.63167113305991));
#9342=CARTESIAN_POINT('Ctrl Pts',(1.11599400238352,28.6027790887188,1.663387589081));
#9343=CARTESIAN_POINT('Ctrl Pts',(1.10936742882001,28.6058862118166,1.66783346591799));
#9344=CARTESIAN_POINT('Ctrl Pts',(1.10271926064605,28.6089862646408,1.67223640644795));
#9345=CARTESIAN_POINT('Ctrl Pts',(1.09605031831593,28.6120789434068,1.6765961304334));
#9346=CARTESIAN_POINT('Ctrl Pts',(1.04927657203313,28.6337699649776,1.70717378629907));
#9347=CARTESIAN_POINT('Ctrl Pts',(1.00096226226722,28.6558246274708,1.73595988153284));
#9348=CARTESIAN_POINT('Ctrl Pts',(0.951326577168889,28.6781333047891,1.76274746587164));
#9349=CARTESIAN_POINT('Ctrl Pts',(0.901757944496797,28.7004118455044,1.78949886308983));
#9350=CARTESIAN_POINT('Ctrl Pts',(0.850871989713288,28.722943462763,1.81425661026415));
#9351=CARTESIAN_POINT('Ctrl Pts',(0.798922307369564,28.7456101450408,1.83685166294178));
#9352=CARTESIAN_POINT('Ctrl Pts',(0.746334656544358,28.768555185688,1.85972419434104));
#9353=CARTESIAN_POINT('Ctrl Pts',(0.692657569252057,28.791638342907,1.88038006400964));
#9354=CARTESIAN_POINT('Ctrl Pts',(0.638182343175099,28.8147322103788,1.89869012261724));
#9355=CARTESIAN_POINT('Ctrl Pts',(0.584378552670652,28.8375414338896,1.91677450020303));
#9356=CARTESIAN_POINT('Ctrl Pts',(0.529796922475223,28.8603608021809,1.93257038955436));
#9357=CARTESIAN_POINT('Ctrl Pts',(0.474735383789332,28.8830671741923,1.94600287775817));
#9358=CARTESIAN_POINT('Ctrl Pts',(0.418643147951686,28.9061985868677,1.95968680875969));
#9359=CARTESIAN_POINT('Ctrl Pts',(0.36205362993619,28.92921241347,1.97091779664273));
#9360=CARTESIAN_POINT('Ctrl Pts',(0.305288522417528,28.9519827968767,1.97967164018299));
#9361=CARTESIAN_POINT('Ctrl Pts',(0.248523414898871,28.9747531802835,1.98842548372325));
#9362=CARTESIAN_POINT('Ctrl Pts',(0.191583499797966,28.9972798392585,1.99470232098375));
#9363=CARTESIAN_POINT('Ctrl Pts',(0.134785361990913,29.019445755387,1.99853290967592));
#9364=CARTESIAN_POINT('Ctrl Pts',(0.126823642527627,29.0225528784843,1.99906986517699));
#9365=CARTESIAN_POINT('Ctrl Pts',(0.118864689736634,29.0256529313079,1.99955883944022));
#9366=CARTESIAN_POINT('Ctrl Pts',(0.11090935427091,29.0287456100735,1.99999999999998));
#9367=CARTESIAN_POINT('Ctrl Pts',(0.0551132738422961,29.0504366316384,2.00309415362558));
#9368=CARTESIAN_POINT('Ctrl Pts',(-0.0011211933826387,29.0724912941254,
2.00386648849128));
#9369=CARTESIAN_POINT('Ctrl Pts',(-0.0575007497658943,29.0947999714375,
2.00224737448728));
#9370=CARTESIAN_POINT('Ctrl Pts',(-0.113804143507052,29.1170785121555,2.00063044773001));
#9371=CARTESIAN_POINT('Ctrl Pts',(-0.170251546639818,29.1396101294169,1.99662830833218));
#9372=CARTESIAN_POINT('Ctrl Pts',(-0.226538817614126,29.1622768116975,1.99022135677887));
#9373=CARTESIAN_POINT('Ctrl Pts',(-0.283517324855257,29.1852218523454,1.98373572460742));
#9374=CARTESIAN_POINT('Ctrl Pts',(-0.340330980887393,29.2083050095649,1.97478568883195));
#9375=CARTESIAN_POINT('Ctrl Pts',(-0.396662939852275,29.2313988770373,1.96340505169272));
#9376=CARTESIAN_POINT('Ctrl Pts',(-0.452300578039161,29.2542081005469,1.95216468684257));
#9377=CARTESIAN_POINT('Ctrl Pts',(-0.507467601041344,29.277027468837,1.93855351319987));
#9378=CARTESIAN_POINT('Ctrl Pts',(-0.561868536414166,29.2997338408473,1.92265561987906));
#9379=CARTESIAN_POINT('Ctrl Pts',(-0.617287803109159,29.3228652535242,1.90646013383096));
#9380=CARTESIAN_POINT('Ctrl Pts',(-0.671911257243838,29.345879080128,1.88789169563894));
#9381=CARTESIAN_POINT('Ctrl Pts',(-0.725448204177296,29.3686494635363,1.86709019276537));
#9382=CARTESIAN_POINT('Ctrl Pts',(-0.778985151110758,29.3914198469445,1.8462886898918));
#9383=CARTESIAN_POINT('Ctrl Pts',(-0.831434982711271,29.413946505921,1.82325463286319));
#9384=CARTESIAN_POINT('Ctrl Pts',(-0.88253890728924,29.4361124220509,1.79817295107712));
#9385=CARTESIAN_POINT('Ctrl Pts',(-0.889702436354912,29.4392195451491,1.7946571084491));
#9386=CARTESIAN_POINT('Ctrl Pts',(-0.896839578793133,29.4423195979737,1.79110109618633));
#9387=CARTESIAN_POINT('Ctrl Pts',(-0.903949681684058,29.4454122767402,1.7875054847043));
#9388=CARTESIAN_POINT('Ctrl Pts',(-0.953817581583688,29.4671032983068,1.76228706013093));
#9389=CARTESIAN_POINT('Ctrl Pts',(-1.00290422620548,29.4891579607957,1.73483868812999));
#9390=CARTESIAN_POINT('Ctrl Pts',(-1.0509207972892,29.5114666381096,1.70524671607653));
#9391=CARTESIAN_POINT('Ctrl Pts',(-1.09887250321126,29.5337451788284,1.67569471955667));
#9392=CARTESIAN_POINT('Ctrl Pts',(-1.1457563186045,29.5562767960907,1.64400506360072));
#9393=CARTESIAN_POINT('Ctrl Pts',(-1.19129904940263,29.5789434783722,1.61031284530589));
#9394=CARTESIAN_POINT('Ctrl Pts',(-1.23740106805556,29.6018885190193,1.57620686946592));
#9395=CARTESIAN_POINT('Ctrl Pts',(-1.28212811957172,29.624971676238,1.54004908310434));
#9396=CARTESIAN_POINT('Ctrl Pts',(-1.32522270850892,29.6480655437097,1.50202718274903));
#9397=CARTESIAN_POINT('Ctrl Pts',(-1.36778613415132,29.6708747672146,1.46447392215491));
#9398=CARTESIAN_POINT('Ctrl Pts',(-1.40875659069272,29.6936941355001,1.42510278851201));
#9399=CARTESIAN_POINT('Ctrl Pts',(-1.44792023604725,29.7164005075058,1.38413434135187));
#9400=CARTESIAN_POINT('Ctrl Pts',(-1.48781698584261,29.7395319201838,1.34239900565837));
#9401=CARTESIAN_POINT('Ctrl Pts',(-1.52583806567193,29.7625457467888,1.29900653940629));
#9402=CARTESIAN_POINT('Ctrl Pts',(-1.56180167032266,29.7853161301982,1.25422343601211));
#9403=CARTESIAN_POINT('Ctrl Pts',(-1.5977652749734,29.8080865136077,1.20944033261793));
#9404=CARTESIAN_POINT('Ctrl Pts',(-1.63167113305121,29.8306131725853,1.1632673382765));
#9405=CARTESIAN_POINT('Ctrl Pts',(-1.66338758907747,29.8527790887163,1.11599400238878));
#9406=CARTESIAN_POINT('Ctrl Pts',(-1.66783346591567,29.8558862118149,1.10936742882351));
#9407=CARTESIAN_POINT('Ctrl Pts',(-1.6722364064468,29.8589862646399,1.1027192606478));
#9408=CARTESIAN_POINT('Ctrl Pts',(-1.67659613043341,29.8620789434068,1.09605031831591));
#9409=CARTESIAN_POINT('Ctrl Pts',(-1.70717378629565,29.8837699649752,1.04927657203835));
#9410=CARTESIAN_POINT('Ctrl Pts',(-1.73595988152635,29.9058246274658,1.0009622622781));
#9411=CARTESIAN_POINT('Ctrl Pts',(-1.76274746586258,29.9281333047816,0.951326577185667));
#9412=CARTESIAN_POINT('Ctrl Pts',(-1.78949886307415,29.9504118454909,0.901757944526982));
#9413=CARTESIAN_POINT('Ctrl Pts',(-1.81425661024294,29.9729434627434,0.850871989757554));
#9414=CARTESIAN_POINT('Ctrl Pts',(-1.83685166291622,29.9956101450151,0.798922307428386));
#9415=CARTESIAN_POINT('Ctrl Pts',(-1.85972419431906,30.0185551856642,0.746334656599543));
#9416=CARTESIAN_POINT('Ctrl Pts',(-1.88038006399093,30.041638342885,0.692657569303313));
#9417=CARTESIAN_POINT('Ctrl Pts',(-1.89869012260142,30.0647322103588,0.638182343222221));
#9418=CARTESIAN_POINT('Ctrl Pts',(-1.91677450018729,30.087541433868,0.584378552721979));
#9419=CARTESIAN_POINT('Ctrl Pts',(-1.93257038953904,30.1103608021577,0.529796922530749));
#9420=CARTESIAN_POINT('Ctrl Pts',(-1.94600287774362,30.1330671741677,0.474735383849046));
#9421=CARTESIAN_POINT('Ctrl Pts',(-1.95968680874906,30.1561985868468,0.418643148002788));
#9422=CARTESIAN_POINT('Ctrl Pts',(-1.97091779663529,30.1792124134529,0.362053629978264));
#9423=CARTESIAN_POINT('Ctrl Pts',(-1.97967164017791,30.2019827968635,0.305288522450557));
#9424=CARTESIAN_POINT('Ctrl Pts',(-1.98842548372053,30.224753180274,0.248523414922854));
#9425=CARTESIAN_POINT('Ctrl Pts',(-1.9947023209826,30.2472798392526,0.191583499812823));
#9426=CARTESIAN_POINT('Ctrl Pts',(-1.99853290967555,30.2694457553847,0.134785361996615));
#9427=CARTESIAN_POINT('Ctrl Pts',(-1.99906986517678,30.2725528784827,0.126823642531405));
#9428=CARTESIAN_POINT('Ctrl Pts',(-1.99955883944014,30.2756529313072,0.118864689738512));
#9429=CARTESIAN_POINT('Ctrl Pts',(-2.,30.2787456100735,0.110909354270867));
#9430=CARTESIAN_POINT('Ctrl Pts',(-2.00309415362522,30.3004366316358,0.0551132738489099));
#9431=CARTESIAN_POINT('Ctrl Pts',(-2.00386648849109,30.3224912941201,-0.00112119336928378));
#9432=CARTESIAN_POINT('Ctrl Pts',(-2.00224737448784,30.3447999714295,-0.0575007497458005));
#9433=CARTESIAN_POINT('Ctrl Pts',(-2.00063044773086,30.3670785121513,-0.113804143496728));
#9434=CARTESIAN_POINT('Ctrl Pts',(-1.99662830833251,30.3896101294167,-0.170251546639406));
#9435=CARTESIAN_POINT('Ctrl Pts',(-1.99022135677783,30.4122768117013,-0.226538817623492));
#9436=CARTESIAN_POINT('Ctrl Pts',(-1.98373572460613,30.4352218523491,-0.283517324864499));
#9437=CARTESIAN_POINT('Ctrl Pts',(-1.9747856888304,30.4583050095686,-0.340330980896505));
#9438=CARTESIAN_POINT('Ctrl Pts',(-1.96340505169093,30.4813988770409,-0.396662939861262));
#9439=CARTESIAN_POINT('Ctrl Pts',(-1.95216468684122,30.5042081005491,-0.452300578044649));
#9440=CARTESIAN_POINT('Ctrl Pts',(-1.93855351319925,30.5270274688378,-0.507467601043391));
#9441=CARTESIAN_POINT('Ctrl Pts',(-1.92265561987947,30.5497338408467,-0.56186853641284));
#9442=CARTESIAN_POINT('Ctrl Pts',(-1.90646013383095,30.5728652535243,-0.617287803109421));
#9443=CARTESIAN_POINT('Ctrl Pts',(-1.88789169563839,30.5958790801287,-0.671911257245612));
#9444=CARTESIAN_POINT('Ctrl Pts',(-1.86709019276414,30.6186494635376,-0.72544820418056));
#9445=CARTESIAN_POINT('Ctrl Pts',(-1.84628868988989,30.6414198469465,-0.778985151115508));
#9446=CARTESIAN_POINT('Ctrl Pts',(-1.82325463286048,30.6639465059236,-0.831434982717405));
#9447=CARTESIAN_POINT('Ctrl Pts',(-1.79817295107351,30.6861124220541,-0.882538907296667));
#9448=CARTESIAN_POINT('Ctrl Pts',(-1.79465710844667,30.6892195451513,-0.889702436359856));
#9449=CARTESIAN_POINT('Ctrl Pts',(-1.79110109618512,30.6923195979748,-0.896839578795616));
#9450=CARTESIAN_POINT('Ctrl Pts',(-1.78750548470434,30.6954122767402,-0.903949681684073));
#9451=CARTESIAN_POINT('Ctrl Pts',(-1.76228706012981,30.7171032983078,-0.953817581585953));
#9452=CARTESIAN_POINT('Ctrl Pts',(-1.73483868812747,30.7391579607977,-1.00290422621001));
#9453=CARTESIAN_POINT('Ctrl Pts',(-1.70524671607249,30.7614666381126,-1.05092079729578));
#9454=CARTESIAN_POINT('Ctrl Pts',(-1.67569471956773,30.78374517882,-1.09887250319292));
#9455=CARTESIAN_POINT('Ctrl Pts',(-1.64400506362909,30.8062767960705,-1.14575631856236));
#9456=CARTESIAN_POINT('Ctrl Pts',(-1.61031284535356,30.8289434783402,-1.19129904933821));
#9457=CARTESIAN_POINT('Ctrl Pts',(-1.57620686951104,30.8518885189901,-1.23740106799845));
#9458=CARTESIAN_POINT('Ctrl Pts',(-1.54004908314627,30.8749716762118,-1.2821281195217));
#9459=CARTESIAN_POINT('Ctrl Pts',(-1.50202718278721,30.8980655436865,-1.32522270846567));
#9460=CARTESIAN_POINT('Ctrl Pts',(-1.46447392219183,30.920874767193,-1.36778613411196));
#9461=CARTESIAN_POINT('Ctrl Pts',(-1.42510278854742,30.9436941354799,-1.40875659065708));
#9462=CARTESIAN_POINT('Ctrl Pts',(-1.38413434138545,30.9664005074872,-1.44792023601518));
#9463=CARTESIAN_POINT('Ctrl Pts',(-1.34239900568604,30.9895319201691,-1.48781698581805));
#9464=CARTESIAN_POINT('Ctrl Pts',(-1.29900653942741,31.0125457467779,-1.52583806565434));
#9465=CARTESIAN_POINT('Ctrl Pts',(-1.25422343602621,31.0353161301911,-1.56180167031137));
#9466=CARTESIAN_POINT('Ctrl Pts',(-1.20944033262501,31.0580865136043,-1.59776527496841));
#9467=CARTESIAN_POINT('Ctrl Pts',(-1.16326733827608,31.0806131725856,-1.63167113305186));
#9468=CARTESIAN_POINT('Ctrl Pts',(-1.11599400238054,31.1027790887202,-1.66338758908304));
#9469=CARTESIAN_POINT('Ctrl Pts',(-1.10936742881802,31.1058862118175,-1.66783346591935));
#9470=CARTESIAN_POINT('Ctrl Pts',(-1.10271926064508,31.1089862646412,-1.67223640644862));
#9471=CARTESIAN_POINT('Ctrl Pts',(-1.09605031831596,31.1120789434068,-1.67659613043341));
#9472=CARTESIAN_POINT('Ctrl Pts',(-1.0492765720558,31.1337699649671,-1.70717378628425));
#9473=CARTESIAN_POINT('Ctrl Pts',(-1.00096226231408,31.1558246274494,-1.73595988150493));
#9474=CARTESIAN_POINT('Ctrl Pts',(-0.951326577241099,31.1781333047567,-1.76274746583267));
#9475=CARTESIAN_POINT('Ctrl Pts',(-0.901757944563462,31.2004118454748,-1.78949886305646));
#9476=CARTESIAN_POINT('Ctrl Pts',(-0.850871989773915,31.2229434627363,-1.81425661023596));
#9477=CARTESIAN_POINT('Ctrl Pts',(-0.798922307423776,31.2456101450171,-1.83685166291821));
#9478=CARTESIAN_POINT('Ctrl Pts',(-0.746334656595517,31.2685551856659,-1.85972419432064));
#9479=CARTESIAN_POINT('Ctrl Pts',(-0.692657569299935,31.2916383428865,-1.88038006399213));
#9480=CARTESIAN_POINT('Ctrl Pts',(-0.638182343219465,31.31473221036,-1.89869012260232));
#9481=CARTESIAN_POINT('Ctrl Pts',(-0.584378552727823,31.3375414338655,-1.91677450018521));
#9482=CARTESIAN_POINT('Ctrl Pts',(-0.529796922545472,31.3603608021516,-1.93257038953474));
#9483=CARTESIAN_POINT('Ctrl Pts',(-0.474735383872727,31.3830671741579,-1.94600287773785));
#9484=CARTESIAN_POINT('Ctrl Pts',(-0.41864314802318,31.4061985868385,-1.95968680874481));
#9485=CARTESIAN_POINT('Ctrl Pts',(-0.36205362999544,31.429212413446,-1.97091779663224));
#9486=CARTESIAN_POINT('Ctrl Pts',(-0.305288522464344,31.451982796858,-1.97967164017579));
#9487=CARTESIAN_POINT('Ctrl Pts',(-0.248523414933249,31.4747531802699,-1.98842548371934));
#9488=CARTESIAN_POINT('Ctrl Pts',(-0.19158349981977,31.4972798392499,-1.99470232098204));
#9489=CARTESIAN_POINT('Ctrl Pts',(-0.134785362000163,31.5194457553834,-1.99853290967532));
#9490=CARTESIAN_POINT('Ctrl Pts',(-0.126823642533793,31.5225528784818,-1.99906986517664));
#9491=CARTESIAN_POINT('Ctrl Pts',(-0.118864689739719,31.5256529313067,-1.99955883944008));
#9492=CARTESIAN_POINT('Ctrl Pts',(-0.110909354270916,31.5287456100735,-2.00000000000001));
#9493=CARTESIAN_POINT('Ctrl Pts',(-0.0551132738398505,31.5504366316393,
-2.00309415362574));
#9494=CARTESIAN_POINT('Ctrl Pts',(0.00112119338755449,31.5724912941273,
-2.00386648849135));
#9495=CARTESIAN_POINT('Ctrl Pts',(0.0575007497732957,31.5947999714404,-2.00224737448707));
#9496=CARTESIAN_POINT('Ctrl Pts',(0.113804143504013,31.6170785121543,-2.00063044772989));
#9497=CARTESIAN_POINT('Ctrl Pts',(0.170251546626252,31.6396101294115,-1.99662830833307));
#9498=CARTESIAN_POINT('Ctrl Pts',(0.226538817590147,31.6622768116879,-1.99022135678163));
#9499=CARTESIAN_POINT('Ctrl Pts',(0.283517324833422,31.6852218523365,-1.98373572461064));
#9500=CARTESIAN_POINT('Ctrl Pts',(0.340330980867798,31.7083050095569,-1.97478568883542));
#9501=CARTESIAN_POINT('Ctrl Pts',(0.396662939834899,31.7313988770301,-1.96340505169626));
#9502=CARTESIAN_POINT('Ctrl Pts',(0.452300578015339,31.7542081005371,-1.95216468684793));
#9503=CARTESIAN_POINT('Ctrl Pts',(0.507467601011179,31.7770274688245,-1.93855351320761));
#9504=CARTESIAN_POINT('Ctrl Pts',(0.561868536377917,31.7997338408322,-1.92265561988969));
#9505=CARTESIAN_POINT('Ctrl Pts',(0.617287803079549,31.8228652535117,-1.90646013384078));
#9506=CARTESIAN_POINT('Ctrl Pts',(0.671911257220686,31.8458790801182,-1.88789169564743));
#9507=CARTESIAN_POINT('Ctrl Pts',(0.725448204160488,31.8686494635291,-1.86709019277195));
#9508=CARTESIAN_POINT('Ctrl Pts',(0.778985151100286,31.89141984694,-1.84628868989648));
#9509=CARTESIAN_POINT('Ctrl Pts',(0.83143498270685,31.9139465059191,-1.82325463286546));
#9510=CARTESIAN_POINT('Ctrl Pts',(0.882538907290595,31.9361124220515,-1.79817295107651));
#9511=CARTESIAN_POINT('Ctrl Pts',(0.889702436355825,31.9392195451495,-1.7946571084487));
#9512=CARTESIAN_POINT('Ctrl Pts',(0.89683957879358,31.9423195979739,-1.79110109618616));
#9513=CARTESIAN_POINT('Ctrl Pts',(0.90394968168406,31.9454122767402,-1.78750548470436));
#9514=CARTESIAN_POINT('Ctrl Pts',(0.953817581579516,31.967103298305,-1.7622870601331));
#9515=CARTESIAN_POINT('Ctrl Pts',(1.0029042261973,31.989157960792,-1.73483868813461));
#9516=CARTESIAN_POINT('Ctrl Pts',(1.0509207972772,32.011466638104,-1.70524671608398));
#9517=CARTESIAN_POINT('Ctrl Pts',(1.09887250319299,32.0337451788198,-1.67569471956845));
#9518=CARTESIAN_POINT('Ctrl Pts',(1.14575631858028,32.056276796079,-1.64400506361739));
#9519=CARTESIAN_POINT('Ctrl Pts',(1.19129904937289,32.0789434783574,-1.61031284532795));
#9520=CARTESIAN_POINT('Ctrl Pts',(1.23740106802881,32.1018885190056,-1.5762068694871));
#9521=CARTESIAN_POINT('Ctrl Pts',(1.28212811954792,32.1249716762256,-1.54004908312433));
#9522=CARTESIAN_POINT('Ctrl Pts',(1.32522270848791,32.1480655436984,-1.50202718276764));
#9523=CARTESIAN_POINT('Ctrl Pts',(1.36778613413943,32.170874767208,-1.46447392216653));
#9524=CARTESIAN_POINT('Ctrl Pts',(1.40875659068932,32.1936941354981,-1.4251027885159));
#9525=CARTESIAN_POINT('Ctrl Pts',(1.44792023605164,32.2164005075084,-1.38413434134735));
#9526=CARTESIAN_POINT('Ctrl Pts',(1.48781698584602,32.2395319201859,-1.34239900565462));
#9527=CARTESIAN_POINT('Ctrl Pts',(1.52583806567441,32.2625457467904,-1.29900653940341));
#9528=CARTESIAN_POINT('Ctrl Pts',(1.56180167032433,32.2853161301994,-1.25422343601012));
#9529=CARTESIAN_POINT('Ctrl Pts',(1.59776527497424,32.3080865136083,-1.20944033261684));
#9530=CARTESIAN_POINT('Ctrl Pts',(1.63167113305132,32.3306131725855,-1.16326733827636));
#9531=CARTESIAN_POINT('Ctrl Pts',(1.66338758907691,32.352779088716,-1.1159940023897));
#9532=CARTESIAN_POINT('Ctrl Pts',(1.6678334659153,32.3558862118148,-1.10936742882416));
#9533=CARTESIAN_POINT('Ctrl Pts',(1.67223640644662,32.3589862646399,-1.10271926064816));
#9534=CARTESIAN_POINT('Ctrl Pts',(1.67659613043341,32.3620789434069,-1.09605031831599));
#9535=CARTESIAN_POINT('Ctrl Pts',(1.70717378628998,32.3837699649712,-1.04927657204709));
#9536=CARTESIAN_POINT('Ctrl Pts',(1.73595988151573,32.4058246274578,-1.00096226229599));
#9537=CARTESIAN_POINT('Ctrl Pts',(1.76274746584775,32.4281333047693,-0.951326577213187));
#9538=CARTESIAN_POINT('Ctrl Pts',(1.78949886306025,32.4504118454787,-0.901757944554595));
#9539=CARTESIAN_POINT('Ctrl Pts',(1.81425661022999,32.4729434627313,-0.850871989785215));
#9540=CARTESIAN_POINT('Ctrl Pts',(1.83685166290423,32.4956101450031,-0.798922307455973));
#9541=CARTESIAN_POINT('Ctrl Pts',(1.8597241943091,32.5185551856534,-0.746334656624628));
#9542=CARTESIAN_POINT('Ctrl Pts',(1.88038006398273,32.5416383428755,-0.692657569325824));
#9543=CARTESIAN_POINT('Ctrl Pts',(1.89869012259478,32.5647322103505,-0.638182343241963));
#9544=CARTESIAN_POINT('Ctrl Pts',(1.91677450017834,32.5875414338561,-0.584378552750432));
#9545=CARTESIAN_POINT('Ctrl Pts',(1.93257038952854,32.6103608021422,-0.529796922568127));
#9546=CARTESIAN_POINT('Ctrl Pts',(1.94600287773232,32.6330671741486,-0.474735383895403));
#9547=CARTESIAN_POINT('Ctrl Pts',(1.95968680874129,32.6561985868315,-0.418643148040505));
#9548=CARTESIAN_POINT('Ctrl Pts',(1.97091779663025,32.6792124134413,-0.362053630007222));
#9549=CARTESIAN_POINT('Ctrl Pts',(1.97967164017484,32.7019827968555,-0.305288522470557));
#9550=CARTESIAN_POINT('Ctrl Pts',(1.98842548371943,32.7247531802696,-0.248523414933892));
#9551=CARTESIAN_POINT('Ctrl Pts',(1.99470232098267,32.7472798392519,-0.191583499814767));
#9552=CARTESIAN_POINT('Ctrl Pts',(1.99853290967603,32.7694457553875,-0.134785361989606));
#9553=CARTESIAN_POINT('Ctrl Pts',(1.99906986517707,32.7725528784846,-0.126823642526751));
#9554=CARTESIAN_POINT('Ctrl Pts',(1.99955883944027,32.7756529313081,-0.118864689736211));
#9555=CARTESIAN_POINT('Ctrl Pts',(2.,32.7787456100735,-0.110909354270917));
#9556=CARTESIAN_POINT('Ctrl Pts',(2.00309415362607,32.8004366316417,-0.0551132738337146));
#9557=CARTESIAN_POINT('Ctrl Pts',(2.00386648849151,32.8224912941322,0.00112119339992733));
#9558=CARTESIAN_POINT('Ctrl Pts',(2.00224737448652,32.8447999714478,0.0575007497919306));
#9559=CARTESIAN_POINT('Ctrl Pts',(2.00063044772872,32.8670785121631,0.113804143526022));
#9560=CARTESIAN_POINT('Ctrl Pts',(1.99662830833099,32.8896101294217,0.170251546651625));
#9561=CARTESIAN_POINT('Ctrl Pts',(1.99022135677835,32.9122768116995,0.226538817618813));
#9562=CARTESIAN_POINT('Ctrl Pts',(1.9837357246068,32.9352218523472,0.283517324859671));
#9563=CARTESIAN_POINT('Ctrl Pts',(1.97478568883126,32.9583050095666,0.34033098089147));
#9564=CARTESIAN_POINT('Ctrl Pts',(1.96340505169196,32.9813988770389,0.396662939856094));
#9565=CARTESIAN_POINT('Ctrl Pts',(1.95216468684278,33.0042081005464,0.452300578037654));
#9566=CARTESIAN_POINT('Ctrl Pts',(1.93855351320149,33.0270274688343,0.50746760103459));
#9567=CARTESIAN_POINT('Ctrl Pts',(1.92265561988254,33.0497338408424,0.56186853640232));
#9568=CARTESIAN_POINT('Ctrl Pts',(1.90646013383411,33.0728652535203,0.617287803099664));
#9569=CARTESIAN_POINT('Ctrl Pts',(1.88789169564162,33.095879080125,0.671911257236546));
#9570=CARTESIAN_POINT('Ctrl Pts',(1.86709019276736,33.1186494635342,0.725448204172222));
#9571=CARTESIAN_POINT('Ctrl Pts',(1.8462886898931,33.1414198469433,0.7789851511079));
#9572=CARTESIAN_POINT('Ctrl Pts',(1.82325463286361,33.1639465059207,0.831434982710542));
#9573=CARTESIAN_POINT('Ctrl Pts',(1.79817295107649,33.1861124220515,0.882538907290563));
#9574=CARTESIAN_POINT('Ctrl Pts',(1.79465710844868,33.1892195451495,0.889702436355792));
#9575=CARTESIAN_POINT('Ctrl Pts',(1.79110109618616,33.1923195979739,0.896839578793529));
#9576=CARTESIAN_POINT('Ctrl Pts',(1.78750548470435,33.1954122767402,0.903949681684009));
#9577=CARTESIAN_POINT('Ctrl Pts',(1.76228706012904,33.2171032983085,0.953817581587484));
#9578=CARTESIAN_POINT('Ctrl Pts',(1.73483868812578,33.2391579607991,1.00290422621303));
#9579=CARTESIAN_POINT('Ctrl Pts',(1.7052467160697,33.2614666381147,1.0509207973003));
#9580=CARTESIAN_POINT('Ctrl Pts',(1.67569471954817,33.2837451788346,1.09887250322439));
#9581=CARTESIAN_POINT('Ctrl Pts',(1.64400506359036,33.306276796098,1.14575631861951));
#9582=CARTESIAN_POINT('Ctrl Pts',(1.61031284529353,33.3289434783805,1.19129904941936));
#9583=CARTESIAN_POINT('Ctrl Pts',(1.57620686945373,33.3518885190272,1.23740106807108));
#9584=CARTESIAN_POINT('Ctrl Pts',(1.54004908309237,33.3749716762455,1.28212811958608));
#9585=CARTESIAN_POINT('Ctrl Pts',(1.5020271827374,33.3980655437167,1.32522270852215));
#9586=CARTESIAN_POINT('Ctrl Pts',(1.46447392213645,33.4208747672256,1.36778613417152));
#9587=CARTESIAN_POINT('Ctrl Pts',(1.42510278848614,33.4436941355149,1.40875659071932));
#9588=CARTESIAN_POINT('Ctrl Pts',(1.38413434131808,33.4664005075245,1.44792023607959));
#9589=CARTESIAN_POINT('Ctrl Pts',(1.34239900562838,33.4895319201999,1.48781698586946));
#9590=CARTESIAN_POINT('Ctrl Pts',(1.2990065393805,33.5125457468022,1.52583806569369));
#9591=CARTESIAN_POINT('Ctrl Pts',(1.25422343599088,33.535316130209,1.56180167033975));
#9592=CARTESIAN_POINT('Ctrl Pts',(1.20944033260126,33.5580865136158,1.59776527498582));
#9593=CARTESIAN_POINT('Ctrl Pts',(1.16326733826477,33.5806131725909,1.63167113305938));
#9594=CARTESIAN_POINT('Ctrl Pts',(1.11599400238226,33.6027790887194,1.66338758908187));
#9595=CARTESIAN_POINT('Ctrl Pts',(1.10936742881915,33.605886211817,1.66783346591858));
#9596=CARTESIAN_POINT('Ctrl Pts',(1.10271926064564,33.6089862646409,1.67223640644824));
#9597=CARTESIAN_POINT('Ctrl Pts',(1.09605031831594,33.6120789434068,1.67659613043342));
#9598=CARTESIAN_POINT('Ctrl Pts',(1.04927657202145,33.633769964983,1.70717378630673));
#9599=CARTESIAN_POINT('Ctrl Pts',(1.00096226224306,33.6558246274818,1.73595988154725));
#9600=CARTESIAN_POINT('Ctrl Pts',(0.951326577131669,33.6781333048059,1.76274746589174));
#9601=CARTESIAN_POINT('Ctrl Pts',(0.9017579444866,33.7004118455088,1.78949886309399));
#9602=CARTESIAN_POINT('Ctrl Pts',(0.850871989731664,33.7229434627548,1.81425661025458));
#9603=CARTESIAN_POINT('Ctrl Pts',(0.798922307417563,33.7456101450198,1.83685166292093));
#9604=CARTESIAN_POINT('Ctrl Pts',(0.74633465658928,33.7685551856686,1.85972419432316));
#9605=CARTESIAN_POINT('Ctrl Pts',(0.692657569293636,33.7916383428892,1.88038006399447));
#9606=CARTESIAN_POINT('Ctrl Pts',(0.638182343213203,33.8147322103626,1.89869012260445));
#9607=CARTESIAN_POINT('Ctrl Pts',(0.584378552714243,33.8375414338713,1.9167745001896));
#9608=CARTESIAN_POINT('Ctrl Pts',(0.529796922524388,33.8603608021604,1.93257038954074));
#9609=CARTESIAN_POINT('Ctrl Pts',(0.474735383844064,33.8830671741698,1.94600287774484));
#9610=CARTESIAN_POINT('Ctrl Pts',(0.41864314799823,33.9061985868487,1.95968680875001));
#9611=CARTESIAN_POINT('Ctrl Pts',(0.362053629974232,33.9292124134546,1.97091779663601));
#9612=CARTESIAN_POINT('Ctrl Pts',(0.305288522446999,33.9519827968649,1.97967164017845));
#9613=CARTESIAN_POINT('Ctrl Pts',(0.248523414919767,33.9747531802752,1.98842548372089));
#9614=CARTESIAN_POINT('Ctrl Pts',(0.191583499810152,33.9972798392537,1.99470232098282));
#9615=CARTESIAN_POINT('Ctrl Pts',(0.134785361994467,34.0194457553856,1.99853290967567));
#9616=CARTESIAN_POINT('Ctrl Pts',(0.126823642529998,34.0225528784833,1.99906986517684));
#9617=CARTESIAN_POINT('Ctrl Pts',(0.118864689737823,34.0256529313075,1.99955883944015));
#9618=CARTESIAN_POINT('Ctrl Pts',(0.110909354270907,34.0287456100735,1.99999999999998));
#9619=CARTESIAN_POINT('Ctrl Pts',(0.0551132738170328,34.0504366316482,2.003094153627));
#9620=CARTESIAN_POINT('Ctrl Pts',(-0.00112119343355195,34.0724912941454,
2.00386648849196));
#9621=CARTESIAN_POINT('Ctrl Pts',(-0.0575007498424811,34.0947999714678,
2.00224737448507));
#9622=CARTESIAN_POINT('Ctrl Pts',(-0.113804143559823,34.1170785121765,2.00063044772634));
#9623=CARTESIAN_POINT('Ctrl Pts',(-0.17025154666847,34.1396101294284,1.99662830832909));
#9624=CARTESIAN_POINT('Ctrl Pts',(-0.226538817618813,34.1622768116994,1.99022135677838));
#9625=CARTESIAN_POINT('Ctrl Pts',(-0.283517324859929,34.1852218523472,1.9837357246068));
#9626=CARTESIAN_POINT('Ctrl Pts',(-0.340330980892099,34.2083050095668,1.97478568883116));
#9627=CARTESIAN_POINT('Ctrl Pts',(-0.396662939856971,34.2313988770392,1.96340505169179));
#9628=CARTESIAN_POINT('Ctrl Pts',(-0.452300578027502,34.2542081005421,1.95216468684481));
#9629=CARTESIAN_POINT('Ctrl Pts',(-0.507467601013651,34.2770274688255,1.93855351320665));
#9630=CARTESIAN_POINT('Ctrl Pts',(-0.561868536370906,34.2997338408293,1.92265561989172));
#9631=CARTESIAN_POINT('Ctrl Pts',(-0.617287803074319,34.3228652535095,1.9064601338425));
#9632=CARTESIAN_POINT('Ctrl Pts',(-0.671911257217177,34.3458790801167,1.88789169564869));
#9633=CARTESIAN_POINT('Ctrl Pts',(-0.725448204158619,34.3686494635283,1.86709019277263));
#9634=CARTESIAN_POINT('Ctrl Pts',(-0.778985151100058,34.3914198469399,1.84628868989658));
#9635=CARTESIAN_POINT('Ctrl Pts',(-0.831434982708242,34.4139465059197,1.82325463286483));
#9636=CARTESIAN_POINT('Ctrl Pts',(-0.88253890729354,34.4361124220528,1.79817295107501));
#9637=CARTESIAN_POINT('Ctrl Pts',(-0.88970243635778,34.4392195451504,1.79465710844767));
#9638=CARTESIAN_POINT('Ctrl Pts',(-0.896839578794564,34.4423195979743,1.79110109618562));
#9639=CARTESIAN_POINT('Ctrl Pts',(-0.903949681684068,34.4454122767402,1.78750548470431));
#9640=CARTESIAN_POINT('Ctrl Pts',(-0.953817581595336,34.4671032983119,1.76228706012506));
#9641=CARTESIAN_POINT('Ctrl Pts',(-1.00290422622842,34.489157960806,1.73483868811717));
#9642=CARTESIAN_POINT('Ctrl Pts',(-1.05092079732283,34.5114666381252,1.70524671605581));
#9643=CARTESIAN_POINT('Ctrl Pts',(-1.09887250321489,34.5337451788305,1.67569471955315));
#9644=CARTESIAN_POINT('Ctrl Pts',(-1.14575631857937,34.5562767960788,1.64400506361705));
#9645=CARTESIAN_POINT('Ctrl Pts',(-1.19129904935051,34.5789434783463,1.61031284534447));
#9646=CARTESIAN_POINT('Ctrl Pts',(-1.237401068009,34.6018885189955,1.57620686950271));
#9647=CARTESIAN_POINT('Ctrl Pts',(-1.28212811953057,34.6249716762165,1.54004908313884));
#9648=CARTESIAN_POINT('Ctrl Pts',(-1.32522270847289,34.6480655436903,1.50202718278086));
#9649=CARTESIAN_POINT('Ctrl Pts',(-1.36778613412684,34.670874767201,1.46447392217835));
#9650=CARTESIAN_POINT('Ctrl Pts',(-1.4087565906791,34.6936941354922,1.42510278852607));
#9651=CARTESIAN_POINT('Ctrl Pts',(-1.44792023604355,34.7164005075036,1.38413434135578));
#9652=CARTESIAN_POINT('Ctrl Pts',(-1.48781698583993,34.7395319201822,1.34239900566143));
#9653=CARTESIAN_POINT('Ctrl Pts',(-1.52583806567025,34.7625457467878,1.29900653940836));
#9654=CARTESIAN_POINT('Ctrl Pts',(-1.56180167032184,34.7853161301977,1.25422343601316));
#9655=CARTESIAN_POINT('Ctrl Pts',(-1.59776527497344,34.8080865136077,1.20944033261796));
#9656=CARTESIAN_POINT('Ctrl Pts',(-1.63167113305207,34.8306131725858,1.16326733827539));
#9657=CARTESIAN_POINT('Ctrl Pts',(-1.66338758907898,34.8527790887174,1.11599400238656));
#9658=CARTESIAN_POINT('Ctrl Pts',(-1.66783346591667,34.8558862118156,1.10936742882202));
#9659=CARTESIAN_POINT('Ctrl Pts',(-1.67223640644732,34.8589862646403,1.10271926064705));
#9660=CARTESIAN_POINT('Ctrl Pts',(-1.67659613043344,34.8620789434068,1.0960503183159));
#9661=CARTESIAN_POINT('Ctrl Pts',(-1.70717378628652,34.8837699649687,1.04927657205235));
#9662=CARTESIAN_POINT('Ctrl Pts',(-1.73595988150919,34.9058246274527,1.00096226230697));
#9663=CARTESIAN_POINT('Ctrl Pts',(-1.76274746583861,34.9281333047616,0.951326577230139));
#9664=CARTESIAN_POINT('Ctrl Pts',(-1.78949886305682,34.9504118454753,0.901757944562123));
#9665=CARTESIAN_POINT('Ctrl Pts',(-1.81425661023148,34.9729434627324,0.850871989782791));
#9666=CARTESIAN_POINT('Ctrl Pts',(-1.83685166290977,34.9956101450087,0.79892230744325));
#9667=CARTESIAN_POINT('Ctrl Pts',(-1.85972419431345,35.0185551856582,0.746334656613635));
#9668=CARTESIAN_POINT('Ctrl Pts',(-1.88038006398612,35.0416383428795,0.692657569316508));
#9669=CARTESIAN_POINT('Ctrl Pts',(-1.89869012259731,35.0647322103537,0.63818234323446));
#9670=CARTESIAN_POINT('Ctrl Pts',(-1.91677450018293,35.0875414338621,0.584378552736114));
#9671=CARTESIAN_POINT('Ctrl Pts',(-1.93257038953459,35.1103608021511,0.529796922546848));
#9672=CARTESIAN_POINT('Ctrl Pts',(-1.94600287773923,35.1330671741603,0.474735383867086));
#9673=CARTESIAN_POINT('Ctrl Pts',(-1.95968680874581,35.1561985868406,0.418643148018389));
#9674=CARTESIAN_POINT('Ctrl Pts',(-1.97091779663295,35.1792124134477,0.362053629991456));
#9675=CARTESIAN_POINT('Ctrl Pts',(-1.97967164017628,35.2019827968593,0.305288522461236));
#9676=CARTESIAN_POINT('Ctrl Pts',(-1.9884254837196,35.2247531802708,0.248523414931019));
#9677=CARTESIAN_POINT('Ctrl Pts',(-1.99470232098214,35.2472798392506,0.191583499818388));
#9678=CARTESIAN_POINT('Ctrl Pts',(-1.99853290967534,35.2694457553837,0.134785361999652));
#9679=CARTESIAN_POINT('Ctrl Pts',(-1.99906986517665,35.2725528784821,0.126823642533447));
#9680=CARTESIAN_POINT('Ctrl Pts',(-1.99955883944008,35.2756529313069,0.118864689739538));
#9681=CARTESIAN_POINT('Ctrl Pts',(-2.,35.2787456100736,0.110909354270899));
#9682=CARTESIAN_POINT('Ctrl Pts',(-2.00309415362537,35.3004366316368,0.0551132738463816));
#9683=CARTESIAN_POINT('Ctrl Pts',(-2.00386648849116,35.3224912941222,-0.00112119337437951));
#9684=CARTESIAN_POINT('Ctrl Pts',(-2.00224737448763,35.3447999714326,-0.057500749753497));
#9685=CARTESIAN_POINT('Ctrl Pts',(-2.00063044773093,35.3670785121475,-0.113804143486897));
#9686=CARTESIAN_POINT('Ctrl Pts',(-1.99662830833435,35.3896101294058,-0.170251546611904));
#9687=CARTESIAN_POINT('Ctrl Pts',(-1.99022135678294,35.4122768116832,-0.22653881757851));
#9688=CARTESIAN_POINT('Ctrl Pts',(-1.98373572461215,35.4352218523323,-0.283517324822981));
#9689=CARTESIAN_POINT('Ctrl Pts',(-1.97478568883704,35.4583050095531,-0.340330980858573));
#9690=CARTESIAN_POINT('Ctrl Pts',(-1.96340505169788,35.4813988770269,-0.396662939826877));
#9691=CARTESIAN_POINT('Ctrl Pts',(-1.95216468684771,35.504208100538,-0.452300578017591));
#9692=CARTESIAN_POINT('Ctrl Pts',(-1.93855351320464,35.5270274688296,-0.507467601023617));
#9693=CARTESIAN_POINT('Ctrl Pts',(-1.92265561988317,35.5497338408415,-0.561868536400175));
#9694=CARTESIAN_POINT('Ctrl Pts',(-1.90646013383459,35.5728652535196,-0.617287803098313));
#9695=CARTESIAN_POINT('Ctrl Pts',(-1.88789169564186,35.5958790801247,-0.671911257236012));
#9696=CARTESIAN_POINT('Ctrl Pts',(-1.8670901927673,35.6186494635342,-0.725448204172447));
#9697=CARTESIAN_POINT('Ctrl Pts',(-1.84628868989274,35.6414198469437,-0.778985151108882));
#9698=CARTESIAN_POINT('Ctrl Pts',(-1.82325463286292,35.6639465059214,-0.831434982712158));
#9699=CARTESIAN_POINT('Ctrl Pts',(-1.7981729510754,35.6861124220525,-0.882538907292838));
#9700=CARTESIAN_POINT('Ctrl Pts',(-1.79465710844794,35.6892195451502,-0.889702436357317));
#9701=CARTESIAN_POINT('Ctrl Pts',(-1.79110109618577,35.6923195979742,-0.896839578794341));
#9702=CARTESIAN_POINT('Ctrl Pts',(-1.78750548470434,35.6954122767402,-0.903949681684091));
#9703=CARTESIAN_POINT('Ctrl Pts',(-1.7622870601352,35.7171032983032,-0.953817581575309));
#9704=CARTESIAN_POINT('Ctrl Pts',(-1.73483868813926,35.7391579607882,-1.00290422618897));
#9705=CARTESIAN_POINT('Ctrl Pts',(-1.7052467160915,35.7614666380983,-1.05092079726496));
#9706=CARTESIAN_POINT('Ctrl Pts',(-1.67569471957129,35.7837451788179,-1.09887250318912));
#9707=CARTESIAN_POINT('Ctrl Pts',(-1.64400506361483,35.8062767960809,-1.14575631858438));
#9708=CARTESIAN_POINT('Ctrl Pts',(-1.61031284531932,35.8289434783632,-1.19129904938451));
#9709=CARTESIAN_POINT('Ctrl Pts',(-1.57620686947829,35.8518885190113,-1.23740106803997));
#9710=CARTESIAN_POINT('Ctrl Pts',(-1.54004908311541,35.8749716762312,-1.28212811955859));
#9711=CARTESIAN_POINT('Ctrl Pts',(-1.50202718275863,35.8980655437039,-1.3252227084981));
#9712=CARTESIAN_POINT('Ctrl Pts',(-1.46447392215545,35.9208747672145,-1.36778613415137));
#9713=CARTESIAN_POINT('Ctrl Pts',(-1.42510278850262,35.9436941355056,-1.40875659070282));
#9714=CARTESIAN_POINT('Ctrl Pts',(-1.38413434133177,35.966400507517,-1.44792023606651));
#9715=CARTESIAN_POINT('Ctrl Pts',(-1.34239900563994,35.9895319201938,-1.48781698585917));
#9716=CARTESIAN_POINT('Ctrl Pts',(-1.29900653938969,36.0125457467975,-1.525838065686));
#9717=CARTESIAN_POINT('Ctrl Pts',(-1.25422343599754,36.0353161302057,-1.56180167033442));
#9718=CARTESIAN_POINT('Ctrl Pts',(-1.20944033260538,36.0580865136139,-1.59776527498283));
#9719=CARTESIAN_POINT('Ctrl Pts',(-1.16326733826615,36.0806131725903,-1.63167113305853));
#9720=CARTESIAN_POINT('Ctrl Pts',(-1.11599400238079,36.1027790887202,-1.66338758908287));
#9721=CARTESIAN_POINT('Ctrl Pts',(-1.10936742881818,36.1058862118175,-1.66783346591924));
#9722=CARTESIAN_POINT('Ctrl Pts',(-1.10271926064514,36.1089862646413,-1.67223640644858));
#9723=CARTESIAN_POINT('Ctrl Pts',(-1.09605031831594,36.1120789434069,-1.67659613043343));
#9724=CARTESIAN_POINT('Ctrl Pts',(-1.04927657205386,36.1337699649681,-1.70717378628555));
#9725=CARTESIAN_POINT('Ctrl Pts',(-1.00096226231002,36.1558246274514,-1.73595988150737));
#9726=CARTESIAN_POINT('Ctrl Pts',(-0.951326577234831,36.1781333047596,-1.76274746583607));
#9727=CARTESIAN_POINT('Ctrl Pts',(-0.90175794458037,36.2004118454672,-1.78949886304713));
#9728=CARTESIAN_POINT('Ctrl Pts',(-0.850871989815301,36.2229434627181,-1.81425661021575));
#9729=CARTESIAN_POINT('Ctrl Pts',(-0.798922307490469,36.2456101449881,-1.83685166288923));
#9730=CARTESIAN_POINT('Ctrl Pts',(-0.746334656657006,36.2685551856395,-1.8597241942962));
#9731=CARTESIAN_POINT('Ctrl Pts',(-0.692657569355879,36.2916383428626,-1.88038006397175));
#9732=CARTESIAN_POINT('Ctrl Pts',(-0.638182343269583,36.3147322103388,-1.8986901225855));
#9733=CARTESIAN_POINT('Ctrl Pts',(-0.584378552779296,36.337541433844,-1.91677450016952));
#9734=CARTESIAN_POINT('Ctrl Pts',(-0.529796922598241,36.3603608021297,-1.93257038952026));
#9735=CARTESIAN_POINT('Ctrl Pts',(-0.474735383926685,36.3830671741357,-1.9460028777247));
#9736=CARTESIAN_POINT('Ctrl Pts',(-0.418643148067304,36.4061985868206,-1.95968680873571));
#9737=CARTESIAN_POINT('Ctrl Pts',(-0.362053630029398,36.4292124134324,-1.97091779662633));
#9738=CARTESIAN_POINT('Ctrl Pts',(-0.305288522488081,36.4519827968485,-1.97967164017215));
#9739=CARTESIAN_POINT('Ctrl Pts',(-0.248523414946763,36.4747531802646,-1.98842548371797));
#9740=CARTESIAN_POINT('Ctrl Pts',(-0.191583499822922,36.4972798392487,-1.99470232098204));
#9741=CARTESIAN_POINT('Ctrl Pts',(-0.134785361993063,36.5194457553861,-1.99853290967581));
#9742=CARTESIAN_POINT('Ctrl Pts',(-0.126823642529047,36.5225528784837,-1.99906986517694));
#9743=CARTESIAN_POINT('Ctrl Pts',(-0.118864689737348,36.5256529313077,-1.99955883944022));
#9744=CARTESIAN_POINT('Ctrl Pts',(-0.110909354270885,36.5287456100735,-2.00000000000002));
#9745=CARTESIAN_POINT('Ctrl Pts',(-0.0551132738534362,36.550436631634,-2.00309415362498));
#9746=CARTESIAN_POINT('Ctrl Pts',(0.00112119336012617,36.5724912941166,
-2.00386648849097));
#9747=CARTESIAN_POINT('Ctrl Pts',(0.0575007497320264,36.5947999714241,-2.00224737448824));
#9748=CARTESIAN_POINT('Ctrl Pts',(0.113804143472436,36.6170785121417,-2.00063044773194));
#9749=CARTESIAN_POINT('Ctrl Pts',(0.170251546604555,36.6396101294028,-1.99662830833518));
#9750=CARTESIAN_POINT('Ctrl Pts',(0.226538817578213,36.6622768116831,-1.99022135678297));
#9751=CARTESIAN_POINT('Ctrl Pts',(0.283517324822228,36.685221852332,-1.98373572461224));
#9752=CARTESIAN_POINT('Ctrl Pts',(0.340330980857321,36.7083050095526,-1.97478568883723));
#9753=CARTESIAN_POINT('Ctrl Pts',(0.396662939825195,36.7313988770262,-1.96340505169821));
#9754=CARTESIAN_POINT('Ctrl Pts',(0.452300578007919,36.754208100534,-1.95216468684971));
#9755=CARTESIAN_POINT('Ctrl Pts',(0.507467601006086,36.7770274688224,-1.93855351320899));
#9756=CARTESIAN_POINT('Ctrl Pts',(0.561868536375043,36.799733840831,-1.92265561989052));
#9757=CARTESIAN_POINT('Ctrl Pts',(0.617287803076668,36.8228652535105,-1.9064601338417));
#9758=CARTESIAN_POINT('Ctrl Pts',(0.671911257217822,36.845879080117,-1.88789169564844));
#9759=CARTESIAN_POINT('Ctrl Pts',(0.725448204157609,36.8686494635279,-1.86709019277307));
#9760=CARTESIAN_POINT('Ctrl Pts',(0.7789851510974,36.8914198469388,-1.84628868989769));
#9761=CARTESIAN_POINT('Ctrl Pts',(0.831434982703969,36.9139465059178,-1.82325463286677));
#9762=CARTESIAN_POINT('Ctrl Pts',(0.882538907287744,36.9361124220503,-1.79817295107791));
#9763=CARTESIAN_POINT('Ctrl Pts',(0.889702436353935,36.9392195451487,-1.79465710844964));
#9764=CARTESIAN_POINT('Ctrl Pts',(0.896839578792637,36.9423195979735,-1.79110109618665));
#9765=CARTESIAN_POINT('Ctrl Pts',(0.903949681684071,36.9454122767402,-1.78750548470436));
#9766=CARTESIAN_POINT('Ctrl Pts',(0.953817581548078,36.9671032982913,-1.76228706014896));
#9767=CARTESIAN_POINT('Ctrl Pts',(1.0029042261354,36.9891579607642,-1.73483868816921));
#9768=CARTESIAN_POINT('Ctrl Pts',(1.05092079718636,37.0114666380618,-1.70524671613992));
#9769=CARTESIAN_POINT('Ctrl Pts',(1.09887250313603,37.0337451787924,-1.67569471960703));
#9770=CARTESIAN_POINT('Ctrl Pts',(1.14575631855595,37.0562767960668,-1.64400506363559));
#9771=CARTESIAN_POINT('Ctrl Pts',(1.19129904937932,37.0789434783606,-1.61031284532312));
#9772=CARTESIAN_POINT('Ctrl Pts',(1.23740106803564,37.1018885190091,-1.57620686948168));
#9773=CARTESIAN_POINT('Ctrl Pts',(1.2821281195551,37.1249716762293,-1.54004908311832));
#9774=CARTESIAN_POINT('Ctrl Pts',(1.32522270849541,37.1480655437024,-1.50202718276097));
#9775=CARTESIAN_POINT('Ctrl Pts',(1.36778613415348,37.1708747672156,-1.46447392215369));
#9776=CARTESIAN_POINT('Ctrl Pts',(1.40875659070937,37.1936941355092,-1.42510278849638));
#9777=CARTESIAN_POINT('Ctrl Pts',(1.44792023607709,37.2164005075231,-1.38413434132068));
#9778=CARTESIAN_POINT('Ctrl Pts',(1.48781698586827,37.2395319201992,-1.34239900562977));
#9779=CARTESIAN_POINT('Ctrl Pts',(1.52583806569367,37.2625457468023,-1.2990065393806));
#9780=CARTESIAN_POINT('Ctrl Pts',(1.56180167034078,37.2853161302098,-1.25422343598961));
#9781=CARTESIAN_POINT('Ctrl Pts',(1.59776527498789,37.3080865136173,-1.20944033259862));
#9782=CARTESIAN_POINT('Ctrl Pts',(1.6316711330624,37.330613172593,-1.16326733826065));
#9783=CARTESIAN_POINT('Ctrl Pts',(1.66338758908568,37.3527790887222,-1.11599400237662));
#9784=CARTESIAN_POINT('Ctrl Pts',(1.66783346592109,37.3558862118188,-1.10936742881541));
#9785=CARTESIAN_POINT('Ctrl Pts',(1.67223640644948,37.3589862646419,-1.10271926064377));
#9786=CARTESIAN_POINT('Ctrl Pts',(1.67659613043341,37.3620789434069,-1.09605031831598));
#9787=CARTESIAN_POINT('Ctrl Pts',(1.70717378627815,37.3837699649629,-1.04927657206516));
#9788=CARTESIAN_POINT('Ctrl Pts',(1.73595988149344,37.4058246274407,-1.0009622623334));
#9789=CARTESIAN_POINT('Ctrl Pts',(1.76274746581662,37.4281333047434,-0.951326577270847));
#9790=CARTESIAN_POINT('Ctrl Pts',(1.78949886303967,37.4504118454601,-0.901757944596598));
#9791=CARTESIAN_POINT('Ctrl Pts',(1.81425661021869,37.4729434627202,-0.850871989810561));
#9792=CARTESIAN_POINT('Ctrl Pts',(1.83685166290074,37.4956101449996,-0.798922307463975));
#9793=CARTESIAN_POINT('Ctrl Pts',(1.85972419430607,37.5185551856502,-0.746334656632202));
#9794=CARTESIAN_POINT('Ctrl Pts',(1.88038006398015,37.5416383428725,-0.692657569332864));
#9795=CARTESIAN_POINT('Ctrl Pts',(1.89869012259259,37.5647322103477,-0.63818234324847));
#9796=CARTESIAN_POINT('Ctrl Pts',(1.91677450017505,37.5875414338517,-0.584378552760858));
#9797=CARTESIAN_POINT('Ctrl Pts',(1.93257038952445,37.6103608021361,-0.529796922582627));
#9798=CARTESIAN_POINT('Ctrl Pts',(1.9460028777278,37.6330671741409,-0.474735383913968));
#9799=CARTESIAN_POINT('Ctrl Pts',(1.95968680873801,37.6561985868251,-0.418643148056295));
#9800=CARTESIAN_POINT('Ctrl Pts',(1.97091779662797,37.6792124134361,-0.362053630020127));
#9801=CARTESIAN_POINT('Ctrl Pts',(1.9796716401733,37.7019827968515,-0.305288522480569));
#9802=CARTESIAN_POINT('Ctrl Pts',(1.98842548371863,37.7247531802668,-0.248523414941015));
#9803=CARTESIAN_POINT('Ctrl Pts',(1.99470232098237,37.7472798392503,-0.191583499818941));
#9804=CARTESIAN_POINT('Ctrl Pts',(1.99853290967595,37.769445755387,-0.134785361990866));
#9805=CARTESIAN_POINT('Ctrl Pts',(1.99906986517703,37.7725528784843,-0.12682364252758));
#9806=CARTESIAN_POINT('Ctrl Pts',(1.99955883944025,37.7756529313079,-0.118864689736665));
#9807=CARTESIAN_POINT('Ctrl Pts',(2.00000000000001,37.7787456100735,-0.110909354270941));
#9808=CARTESIAN_POINT('Ctrl Pts',(2.00309415362695,37.8004366316478,-0.0551132738181009));
#9809=CARTESIAN_POINT('Ctrl Pts',(2.00386648849195,37.8224912941446,0.00112119343143236));
#9810=CARTESIAN_POINT('Ctrl Pts',(2.00224737448518,37.8447999714666,0.0575007498392763));
#9811=CARTESIAN_POINT('Ctrl Pts',(2.00063044772644,37.8670785121765,0.113804143559674));
#9812=CARTESIAN_POINT('Ctrl Pts',(1.99662830832893,37.8896101294297,0.170251546671467));
#9813=CARTESIAN_POINT('Ctrl Pts',(1.9902213567777,37.9122768117019,0.226538817624831));
#9814=CARTESIAN_POINT('Ctrl Pts',(1.98373572460605,37.9352218523494,0.283517324865039));
#9815=CARTESIAN_POINT('Ctrl Pts',(1.97478568883041,37.9583050095686,0.340330980896365));
#9816=CARTESIAN_POINT('Ctrl Pts',(1.96340505169111,37.9813988770406,0.396662939860387));
#9817=CARTESIAN_POINT('Ctrl Pts',(1.95216468684383,38.004208100544,0.452300578031931));
#9818=CARTESIAN_POINT('Ctrl Pts',(1.93855351320529,38.0270274688278,0.507467601019013));
#9819=CARTESIAN_POINT('Ctrl Pts',(1.9226556198899,38.0497338408319,0.561868536377183));
#9820=CARTESIAN_POINT('Ctrl Pts',(1.90646013384102,38.0728652535115,0.617287803078779));
#9821=CARTESIAN_POINT('Ctrl Pts',(1.8878916956477,38.0958790801179,0.671911257219888));
#9822=CARTESIAN_POINT('Ctrl Pts',(1.86709019277227,38.1186494635288,0.725448204159634));
#9823=CARTESIAN_POINT('Ctrl Pts',(1.84628868989685,38.1414198469397,0.778985151099376));
#9824=CARTESIAN_POINT('Ctrl Pts',(1.82325463286587,38.1639465059187,0.831434982705915));
#9825=CARTESIAN_POINT('Ctrl Pts',(1.79817295107695,38.1861124220511,0.882538907289653));
#9826=CARTESIAN_POINT('Ctrl Pts',(1.79465710844899,38.1892195451493,0.889702436355193));
#9827=CARTESIAN_POINT('Ctrl Pts',(1.7911010961863,38.1923195979738,0.896839578793259));
#9828=CARTESIAN_POINT('Ctrl Pts',(1.78750548470435,38.1954122767402,0.903949681684035));
#9829=CARTESIAN_POINT('Ctrl Pts',(1.76228706013013,38.2171032983075,0.953817581585345));
#9830=CARTESIAN_POINT('Ctrl Pts',(1.7348386881282,38.2391579607971,1.00290422620872));
#9831=CARTESIAN_POINT('Ctrl Pts',(1.70524671607363,38.2614666381118,1.05092079729395));
#9832=CARTESIAN_POINT('Ctrl Pts',(1.67569471955799,38.2837451788273,1.09887250320886));
#9833=CARTESIAN_POINT('Ctrl Pts',(1.64400506360691,38.3062767960863,1.14575631859525));
#9834=CARTESIAN_POINT('Ctrl Pts',(1.61031284531752,38.3289434783644,1.19129904938695));
#9835=CARTESIAN_POINT('Ctrl Pts',(1.57620686947642,38.3518885190125,1.23740106804235));
#9836=CARTESIAN_POINT('Ctrl Pts',(1.54004908311345,38.3749716762323,1.28212811956094));
#9837=CARTESIAN_POINT('Ctrl Pts',(1.50202718275659,38.3980655437051,1.3252227085004));
#9838=CARTESIAN_POINT('Ctrl Pts',(1.46447392215405,38.4208747672153,1.36778613415282));
#9839=CARTESIAN_POINT('Ctrl Pts',(1.42510278850193,38.443694135506,1.40875659070347));
#9840=CARTESIAN_POINT('Ctrl Pts',(1.38413434133184,38.4664005075169,1.44792023606643));
#9841=CARTESIAN_POINT('Ctrl Pts',(1.3423990056396,38.4895319201939,1.48781698585948));
#9842=CARTESIAN_POINT('Ctrl Pts',(1.29900653938895,38.5125457467979,1.52583806568664));
#9843=CARTESIAN_POINT('Ctrl Pts',(1.25422343599634,38.5353161302063,1.56180167033536));
#9844=CARTESIAN_POINT('Ctrl Pts',(1.20944033260373,38.5580865136147,1.59776527498408));
#9845=CARTESIAN_POINT('Ctrl Pts',(1.16326733826403,38.5806131725914,1.63167113306004));
#9846=CARTESIAN_POINT('Ctrl Pts',(1.11599400237818,38.6027790887214,1.6633875890846));
#9847=CARTESIAN_POINT('Ctrl Pts',(1.10936742881645,38.6058862118183,1.66783346592037));
#9848=CARTESIAN_POINT('Ctrl Pts',(1.10271926064427,38.6089862646417,1.67223640644913));
#9849=CARTESIAN_POINT('Ctrl Pts',(1.09605031831595,38.6120789434069,1.6765961304334));
#9850=CARTESIAN_POINT('Ctrl Pts',(1.0492765720158,38.6337699649858,1.70717378631043));
#9851=CARTESIAN_POINT('Ctrl Pts',(1.00096226223136,38.6558246274873,1.73595988155423));
#9852=CARTESIAN_POINT('Ctrl Pts',(0.951326577113638,38.6781333048141,1.76274746590148));
#9853=CARTESIAN_POINT('Ctrl Pts',(0.901757944475194,38.700411845514,1.7894988630995));
#9854=CARTESIAN_POINT('Ctrl Pts',(0.850871989727273,38.7229434627568,1.8142566102564));
#9855=CARTESIAN_POINT('Ctrl Pts',(0.798922307420521,38.7456101450186,1.83685166291966));
#9856=CARTESIAN_POINT('Ctrl Pts',(0.746334656591805,38.7685551856676,1.85972419432218));
#9857=CARTESIAN_POINT('Ctrl Pts',(0.692657569295748,38.7916383428884,1.88038006399372));
#9858=CARTESIAN_POINT('Ctrl Pts',(0.638182343214835,38.814732210362,1.89869012260392));
#9859=CARTESIAN_POINT('Ctrl Pts',(0.584378552717411,38.83754143387,1.9167745001886));
#9860=CARTESIAN_POINT('Ctrl Pts',(0.529796922529156,38.8603608021585,1.93257038953941));
#9861=CARTESIAN_POINT('Ctrl Pts',(0.474735383850398,38.8830671741672,1.94600287774331));
#9862=CARTESIAN_POINT('Ctrl Pts',(0.41864314800303,38.9061985868468,1.95968680874905));
#9863=CARTESIAN_POINT('Ctrl Pts',(0.362053629977474,38.9292124134533,1.97091779663548));
#9864=CARTESIAN_POINT('Ctrl Pts',(0.305288522448675,38.9519827968643,1.97967164017821));
#9865=CARTESIAN_POINT('Ctrl Pts',(0.248523414919876,38.9747531802752,1.98842548372094));
#9866=CARTESIAN_POINT('Ctrl Pts',(0.191583499808698,38.9972798392543,1.99470232098303));
#9867=CARTESIAN_POINT('Ctrl Pts',(0.1347853619914,39.0194457553868,1.9985329096759));
#9868=CARTESIAN_POINT('Ctrl Pts',(0.126823642527947,39.0225528784841,1.99906986517699));
#9869=CARTESIAN_POINT('Ctrl Pts',(0.118864689736811,39.0256529313079,1.99955883944023));
#9870=CARTESIAN_POINT('Ctrl Pts',(0.110909354270921,39.0287456100735,2.));
#9871=CARTESIAN_POINT('Ctrl Pts',(0.0551132738216044,39.0504366316464,2.00309415362675));
#9872=CARTESIAN_POINT('Ctrl Pts',(-0.00112119342432845,39.0724912941418,
2.00386648849185));
#9873=CARTESIAN_POINT('Ctrl Pts',(-0.0575007498285725,39.0947999714623,
2.00224737448548));
#9874=CARTESIAN_POINT('Ctrl Pts',(-0.113804143544574,39.1170785121705,2.00063044772717));
#9875=CARTESIAN_POINT('Ctrl Pts',(-0.170251546651944,39.1396101294219,1.99662830833046));
#9876=CARTESIAN_POINT('Ctrl Pts',(-0.226538817601016,39.1622768116923,1.9902213567804));
#9877=CARTESIAN_POINT('Ctrl Pts',(-0.283517324843828,39.1852218523408,1.98373572460914));
#9878=CARTESIAN_POINT('Ctrl Pts',(-0.340330980877668,39.2083050095609,1.97478568883371));
#9879=CARTESIAN_POINT('Ctrl Pts',(-0.396662939844236,39.231398877034,1.96340505169437));
#9880=CARTESIAN_POINT('Ctrl Pts',(-0.452300578025572,39.2542081005414,1.95216468684558));
#9881=CARTESIAN_POINT('Ctrl Pts',(-0.507467601022369,39.2770274688292,1.93855351320469));
#9882=CARTESIAN_POINT('Ctrl Pts',(-0.561868536389967,39.2997338408373,1.92265561988615));
#9883=CARTESIAN_POINT('Ctrl Pts',(-0.617287803090361,39.3228652535163,1.90646013383722));
#9884=CARTESIAN_POINT('Ctrl Pts',(-0.671911257230311,39.3458790801223,1.88789169564393));
#9885=CARTESIAN_POINT('Ctrl Pts',(-0.725448204168872,39.3686494635327,1.86709019276865));
#9886=CARTESIAN_POINT('Ctrl Pts',(-0.778985151107431,39.3914198469431,1.84628868989338));
#9887=CARTESIAN_POINT('Ctrl Pts',(-0.831434982712827,39.4139465059217,1.82325463286265));
#9888=CARTESIAN_POINT('Ctrl Pts',(-0.882538907295425,39.4361124220536,1.79817295107409));
#9889=CARTESIAN_POINT('Ctrl Pts',(-0.889702436359024,39.4392195451509,1.79465710844706));
#9890=CARTESIAN_POINT('Ctrl Pts',(-0.896839578795191,39.4423195979746,1.7911010961853));
#9891=CARTESIAN_POINT('Ctrl Pts',(-0.903949681684063,39.4454122767402,1.78750548470431));
#9892=CARTESIAN_POINT('Ctrl Pts',(-0.953817581594742,39.4671032983116,1.76228706012535));
#9893=CARTESIAN_POINT('Ctrl Pts',(-1.00290422622729,39.4891579608055,1.73483868811778));
#9894=CARTESIAN_POINT('Ctrl Pts',(-1.0509207973212,39.5114666381245,1.7052467160568));
#9895=CARTESIAN_POINT('Ctrl Pts',(-1.09887250321436,39.5337451788302,1.67569471955352));
#9896=CARTESIAN_POINT('Ctrl Pts',(-1.14575631857987,39.5562767960791,1.64400506361672));
#9897=CARTESIAN_POINT('Ctrl Pts',(-1.191299049352,39.578943478347,1.61031284534333));
#9898=CARTESIAN_POINT('Ctrl Pts',(-1.23740106801089,39.6018885189965,1.5762068695012));
#9899=CARTESIAN_POINT('Ctrl Pts',(-1.28212811953282,39.6249716762176,1.54004908313695));
#9900=CARTESIAN_POINT('Ctrl Pts',(-1.32522270847548,39.6480655436917,1.50202718277854));
#9901=CARTESIAN_POINT('Ctrl Pts',(-1.36778613413884,39.6708747672075,1.4644739221676));
#9902=CARTESIAN_POINT('Ctrl Pts',(-1.40875659069979,39.6936941355038,1.42510278850608));
#9903=CARTESIAN_POINT('Ctrl Pts',(-1.44792023607208,39.7164005075202,1.38413434132589));
#9904=CARTESIAN_POINT('Ctrl Pts',(-1.48781698586376,39.7395319201965,1.34239900563475));
#9905=CARTESIAN_POINT('Ctrl Pts',(-1.52583806568971,39.7625457467998,1.29900653938524));
#9906=CARTESIAN_POINT('Ctrl Pts',(-1.56180167033728,39.7853161302076,1.25422343599392));
#9907=CARTESIAN_POINT('Ctrl Pts',(-1.59776527498484,39.8080865136153,1.2094403326026));
#9908=CARTESIAN_POINT('Ctrl Pts',(-1.63167113305979,39.8306131725912,1.16326733826427));
#9909=CARTESIAN_POINT('Ctrl Pts',(-1.66338758908347,39.8527790887206,1.11599400237985));
#9910=CARTESIAN_POINT('Ctrl Pts',(-1.66783346591964,39.8558862118178,1.10936742881753));
#9911=CARTESIAN_POINT('Ctrl Pts',(-1.67223640644877,39.8589862646414,1.10271926064481));
#9912=CARTESIAN_POINT('Ctrl Pts',(-1.67659613043342,39.8620789434069,1.09605031831591));
#9913=CARTESIAN_POINT('Ctrl Pts',(-1.70717378631508,39.883769964989,1.04927657200867));
#9914=CARTESIAN_POINT('Ctrl Pts',(-1.73595988156297,39.905824627494,1.00096226221665));
#9915=CARTESIAN_POINT('Ctrl Pts',(-1.76274746591369,39.9281333048242,0.951326577090993));
#9916=CARTESIAN_POINT('Ctrl Pts',(-1.78949886311837,39.9504118455302,0.901757944438676));
#9917=CARTESIAN_POINT('Ctrl Pts',(-1.81425661028082,39.9729434627793,0.850871989676198));
#9918=CARTESIAN_POINT('Ctrl Pts',(-1.8368516629484,39.9956101450475,0.798922307354412));
#9919=CARTESIAN_POINT('Ctrl Pts',(-1.85972419434675,40.0185551856943,0.746334656530118));
#9920=CARTESIAN_POINT('Ctrl Pts',(-1.88038006401451,40.0416383429127,0.69265756923881));
#9921=CARTESIAN_POINT('Ctrl Pts',(-1.89869012262136,40.064732210384,0.638182343162886));
#9922=CARTESIAN_POINT('Ctrl Pts',(-1.91677450020403,40.0875414338913,0.58437855266658));
#9923=CARTESIAN_POINT('Ctrl Pts',(-1.93257038955292,40.1103608021791,0.529796922479594));
#9924=CARTESIAN_POINT('Ctrl Pts',(-1.94600287775504,40.133067174187,0.474735383802248));
#9925=CARTESIAN_POINT('Ctrl Pts',(-1.95968680875752,40.1561985868634,0.418643147962249));
#9926=CARTESIAN_POINT('Ctrl Pts',(-1.97091779664134,40.1792124134667,0.362053629944233));
#9927=CARTESIAN_POINT('Ctrl Pts',(-1.97967164018214,40.2019827968745,0.305288522423077));
#9928=CARTESIAN_POINT('Ctrl Pts',(-1.98842548372294,40.2247531802823,0.248523414901921));
#9929=CARTESIAN_POINT('Ctrl Pts',(-1.99470232098377,40.2472798392583,0.191583499798515));
#9930=CARTESIAN_POINT('Ctrl Pts',(-1.99853290967604,40.2694457553877,0.134785361988986));
#9931=CARTESIAN_POINT('Ctrl Pts',(-1.99906986517707,40.2725528784847,0.126823642526306));
#9932=CARTESIAN_POINT('Ctrl Pts',(-1.99955883944026,40.2756529313082,0.118864689735964));
#9933=CARTESIAN_POINT('Ctrl Pts',(-1.99999999999998,40.2787456100735,0.110909354270834));
#9934=CARTESIAN_POINT('Origin',(-2.00026128978551,0.00614793747541198,0.00052367985300868));
#9935=CARTESIAN_POINT('Origin',(-2.,39.7212543899267,-0.110909354270917));
#9936=CARTESIAN_POINT('Origin',(-1.99999999999999,40.0000000000001,-7.63278329429795E-14));
#9937=CARTESIAN_POINT('',(-1.74999999999999,39.9999999999897,-4.17027523624824E-12));
#9938=CARTESIAN_POINT('',(-1.99999999998663,40.0000000000001,-7.63278329429795E-14));
#9939=CARTESIAN_POINT('Origin',(-2.00046279962269,40.0004045588857,0.000160968866383087));
#9940=CARTESIAN_POINT('Origin',(-2.,-0.27874561007344,-0.110909354270924));
#9941=CARTESIAN_POINT('',(-2.28755052096797,0.0795884994942361,0.0313009478093308));
#9942=CARTESIAN_POINT('',(-1.91825489052517,-0.0225146681393854,-0.00895830181614488));
#9943=CARTESIAN_POINT('Origin',(-2.,-2.08166817117217E-14,-3.46944695195361E-14));
#9944=CARTESIAN_POINT('Ctrl Pts',(-2.,0.278745610073468,0.110909354270813));
#9945=CARTESIAN_POINT('Ctrl Pts',(-2.02971807190995,0.487078943406699,-0.424989030591362));
#9946=CARTESIAN_POINT('Ctrl Pts',(-1.78750548470433,0.695412276740089,-0.90394968168412));
#9947=CARTESIAN_POINT('Ctrl Pts',(-1.54529289749872,0.903745610073333,-1.3829103327768));
#9948=CARTESIAN_POINT('Ctrl Pts',(-1.09605031831593,1.11207894340676,-1.67659613043348));
#9949=CARTESIAN_POINT('Ctrl Pts',(-0.646807739133152,1.32041227674011,-1.97028192809006));
#9950=CARTESIAN_POINT('Ctrl Pts',(-0.110909354270893,1.52874561007344,-2.00000000000001));
#9951=CARTESIAN_POINT('Ctrl Pts',(0.42498903059134,1.7370789434067,-2.02971807190998));
#9952=CARTESIAN_POINT('Ctrl Pts',(0.903949681684066,1.94541227674011,-1.78750548470433));
#9953=CARTESIAN_POINT('Ctrl Pts',(1.38291033277679,2.15374561007344,-1.54529289749872));
#9954=CARTESIAN_POINT('Ctrl Pts',(1.67659613043343,2.36207894340677,-1.09605031831594));
#9955=CARTESIAN_POINT('Ctrl Pts',(1.97028192809005,2.57041227674009,-0.646807739133166));
#9956=CARTESIAN_POINT('Ctrl Pts',(2.00000000000003,2.77874561007344,-0.110909354270911));
#9957=CARTESIAN_POINT('Ctrl Pts',(2.02971807190995,2.98707894340676,0.424989030591319));
#9958=CARTESIAN_POINT('Ctrl Pts',(1.78750548470433,3.1954122767401,0.903949681684016));
#9959=CARTESIAN_POINT('Ctrl Pts',(1.54529289749872,3.40374561007338,1.38291033277678));
#9960=CARTESIAN_POINT('Ctrl Pts',(1.09605031831593,3.61207894340677,1.67659613043342));
#9961=CARTESIAN_POINT('Ctrl Pts',(0.646807739133154,3.82041227674006,1.97028192809004));
#9962=CARTESIAN_POINT('Ctrl Pts',(0.110909354270907,4.02874561007344,1.99999999999995));
#9963=CARTESIAN_POINT('Ctrl Pts',(-0.424989030591324,4.23707894340672,2.02971807190993));
#9964=CARTESIAN_POINT('Ctrl Pts',(-0.903949681684066,4.44541227674011,1.78750548470433));
#9965=CARTESIAN_POINT('Ctrl Pts',(-1.38291033277679,4.65374561007344,1.54529289749866));
#9966=CARTESIAN_POINT('Ctrl Pts',(-1.67659613043344,4.8620789434068,1.09605031831587));
#9967=CARTESIAN_POINT('Ctrl Pts',(-1.97028192809005,5.07041227674005,0.646807739133138));
#9968=CARTESIAN_POINT('Ctrl Pts',(-2.,5.27874561007342,0.110909354270813));
#9969=CARTESIAN_POINT('Ctrl Pts',(-2.02971807190995,5.48707894340671,-0.424989030591405));
#9970=CARTESIAN_POINT('Ctrl Pts',(-1.78750548470433,5.6954122767401,-0.90394968168412));
#9971=CARTESIAN_POINT('Ctrl Pts',(-1.54529289749872,5.90374561007338,-1.38291033277678));
#9972=CARTESIAN_POINT('Ctrl Pts',(-1.09605031831592,6.11207894340678,-1.67659613043342));
#9973=CARTESIAN_POINT('Ctrl Pts',(-0.646807739133139,6.3204122767401,-1.97028192809006));
#9974=CARTESIAN_POINT('Ctrl Pts',(-0.110909354270905,6.52874561007347,-2.00000000000006));
#9975=CARTESIAN_POINT('Ctrl Pts',(0.424989030591338,6.73707894340672,-2.02971807190996));
#9976=CARTESIAN_POINT('Ctrl Pts',(0.903949681684068,6.94541227674014,-1.78750548470433));
#9977=CARTESIAN_POINT('Ctrl Pts',(1.38291033277681,7.15374561007342,-1.54529289749877));
#9978=CARTESIAN_POINT('Ctrl Pts',(1.6765961304334,7.36207894340677,-1.09605031831599));
#9979=CARTESIAN_POINT('Ctrl Pts',(1.97028192809006,7.57041227674011,-0.646807739133152));
#9980=CARTESIAN_POINT('Ctrl Pts',(2.,7.77874561007349,-0.110909354270917));
#9981=CARTESIAN_POINT('Ctrl Pts',(2.02971807190995,7.98707894340672,0.424989030591319));
#9982=CARTESIAN_POINT('Ctrl Pts',(1.78750548470433,8.19541227674012,0.903949681684058));
#9983=CARTESIAN_POINT('Ctrl Pts',(1.54529289749873,8.40374561007341,1.3829103327768));
#9984=CARTESIAN_POINT('Ctrl Pts',(1.09605031831593,8.6120789434068,1.67659613043337));
#9985=CARTESIAN_POINT('Ctrl Pts',(0.646807739133154,8.82041227674011,1.97028192809005));
#9986=CARTESIAN_POINT('Ctrl Pts',(0.110909354270904,9.02874561007346,1.99999999999994));
#9987=CARTESIAN_POINT('Ctrl Pts',(-0.424989030591337,9.23707894340678,2.02971807190995));
#9988=CARTESIAN_POINT('Ctrl Pts',(-0.903949681684064,9.44541227674011,1.78750548470427));
#9989=CARTESIAN_POINT('Ctrl Pts',(-1.38291033277679,9.65374561007344,1.54529289749871));
#9990=CARTESIAN_POINT('Ctrl Pts',(-1.67659613043342,9.86207894340678,1.09605031831593));
#9991=CARTESIAN_POINT('Ctrl Pts',(-1.97028192809005,10.0704122767401,0.646807739133152));
#9992=CARTESIAN_POINT('Ctrl Pts',(-1.99999999999999,10.2787456100735,0.110909354270841));
#9993=CARTESIAN_POINT('Ctrl Pts',(-2.02971807190994,10.4870789434068,-0.42498903059134));
#9994=CARTESIAN_POINT('Ctrl Pts',(-1.78750548470433,10.6954122767401,-0.903949681684169));
#9995=CARTESIAN_POINT('Ctrl Pts',(-1.54529289749871,10.9037456100734,-1.38291033277681));
#9996=CARTESIAN_POINT('Ctrl Pts',(-1.09605031831593,11.1120789434068,-1.67659613043348));
#9997=CARTESIAN_POINT('Ctrl Pts',(-0.646807739133152,11.3204122767401,-1.97028192809006));
#9998=CARTESIAN_POINT('Ctrl Pts',(-0.110909354270907,11.5287456100735,-2.00000000000002));
#9999=CARTESIAN_POINT('Ctrl Pts',(0.424989030591338,11.7370789434068,-2.02971807190997));
#10000=CARTESIAN_POINT('Ctrl Pts',(0.903949681684066,11.9454122767401,-1.78750548470433));
#10001=CARTESIAN_POINT('Ctrl Pts',(1.3829103327768,12.1537456100734,-1.54529289749877));
#10002=CARTESIAN_POINT('Ctrl Pts',(1.67659613043342,12.3620789434068,-1.09605031831594));
#10003=CARTESIAN_POINT('Ctrl Pts',(1.97028192809008,12.5704122767401,-0.646807739133166));
#10004=CARTESIAN_POINT('Ctrl Pts',(2.,12.7787456100735,-0.110909354270959));
#10005=CARTESIAN_POINT('Ctrl Pts',(2.02971807190995,12.9870789434068,0.42498903059134));
#10006=CARTESIAN_POINT('Ctrl Pts',(1.78750548470433,13.1954122767401,0.903949681684009));
#10007=CARTESIAN_POINT('Ctrl Pts',(1.54529289749872,13.4037456100734,1.38291033277679));
#10008=CARTESIAN_POINT('Ctrl Pts',(1.09605031831593,13.6120789434068,1.67659613043342));
#10009=CARTESIAN_POINT('Ctrl Pts',(0.646807739133154,13.8204122767401,1.97028192809006));
#10010=CARTESIAN_POINT('Ctrl Pts',(0.110909354270907,14.0287456100735,1.99999999999997));
#10011=CARTESIAN_POINT('Ctrl Pts',(-0.424989030591338,14.2370789434068,
2.02971807190995));
#10012=CARTESIAN_POINT('Ctrl Pts',(-0.903949681684066,14.4454122767402,
1.78750548470424));
#10013=CARTESIAN_POINT('Ctrl Pts',(-1.38291033277679,14.6537456100734,1.54529289749866));
#10014=CARTESIAN_POINT('Ctrl Pts',(-1.67659613043342,14.8620789434068,1.09605031831587));
#10015=CARTESIAN_POINT('Ctrl Pts',(-1.97028192809004,15.0704122767401,0.646807739133166));
#10016=CARTESIAN_POINT('Ctrl Pts',(-2.,15.2787456100735,0.110909354270848));
#10017=CARTESIAN_POINT('Ctrl Pts',(-2.02971807190995,15.4870789434068,-0.424989030591448));
#10018=CARTESIAN_POINT('Ctrl Pts',(-1.78750548470433,15.6954122767401,-0.903949681684079));
#10019=CARTESIAN_POINT('Ctrl Pts',(-1.54529289749872,15.9037456100734,-1.3829103327768));
#10020=CARTESIAN_POINT('Ctrl Pts',(-1.09605031831592,16.1120789434068,-1.67659613043346));
#10021=CARTESIAN_POINT('Ctrl Pts',(-0.646807739133152,16.3204122767401,
-1.97028192809011));
#10022=CARTESIAN_POINT('Ctrl Pts',(-0.110909354270907,16.5287456100735,
-2.00000000000005));
#10023=CARTESIAN_POINT('Ctrl Pts',(0.42498903059134,16.7370789434068,-2.02971807190995));
#10024=CARTESIAN_POINT('Ctrl Pts',(0.90394968168408,16.9454122767401,-1.78750548470433));
#10025=CARTESIAN_POINT('Ctrl Pts',(1.38291033277679,17.1537456100734,-1.54529289749872));
#10026=CARTESIAN_POINT('Ctrl Pts',(1.67659613043342,17.3620789434068,-1.09605031831599));
#10027=CARTESIAN_POINT('Ctrl Pts',(1.97028192809005,17.5704122767401,-0.646807739133152));
#10028=CARTESIAN_POINT('Ctrl Pts',(2.,17.7787456100735,-0.110909354270917));
#10029=CARTESIAN_POINT('Ctrl Pts',(2.02971807190995,17.9870789434068,0.424989030591283));
#10030=CARTESIAN_POINT('Ctrl Pts',(1.78750548470433,18.1954122767401,0.903949681684051));
#10031=CARTESIAN_POINT('Ctrl Pts',(1.54529289749873,18.4037456100734,1.3829103327768));
#10032=CARTESIAN_POINT('Ctrl Pts',(1.09605031831593,18.6120789434068,1.67659613043337));
#10033=CARTESIAN_POINT('Ctrl Pts',(0.646807739133154,18.8204122767401,1.97028192809005));
#10034=CARTESIAN_POINT('Ctrl Pts',(0.110909354270905,19.0287456100735,1.99999999999995));
#10035=CARTESIAN_POINT('Ctrl Pts',(-0.424989030591338,19.2370789434068,
2.02971807190995));
#10036=CARTESIAN_POINT('Ctrl Pts',(-0.903949681684064,19.4454122767402,
1.78750548470426));
#10037=CARTESIAN_POINT('Ctrl Pts',(-1.38291033277679,19.6537456100734,1.54529289749871));
#10038=CARTESIAN_POINT('Ctrl Pts',(-1.67659613043342,19.8620789434068,1.0960503183159));
#10039=CARTESIAN_POINT('Ctrl Pts',(-1.97028192809006,20.0704122767401,0.646807739133152));
#10040=CARTESIAN_POINT('Ctrl Pts',(-1.99999999999999,20.2787456100735,0.11090935427082));
#10041=CARTESIAN_POINT('Ctrl Pts',(-2.02971807190993,20.4870789434068,-0.424989030591398));
#10042=CARTESIAN_POINT('Ctrl Pts',(-1.78750548470433,20.6954122767402,-0.903949681684127));
#10043=CARTESIAN_POINT('Ctrl Pts',(-1.5452928974987,20.9037456100735,-1.38291033277683));
#10044=CARTESIAN_POINT('Ctrl Pts',(-1.09605031831595,21.1120789434068,-1.67659613043348));
#10045=CARTESIAN_POINT('Ctrl Pts',(-0.646807739133154,21.3204122767401,
-1.97028192809006));
#10046=CARTESIAN_POINT('Ctrl Pts',(-0.110909354270907,21.5287456100735,
-2.));
#10047=CARTESIAN_POINT('Ctrl Pts',(0.424989030591338,21.7370789434068,-2.02971807190994));
#10048=CARTESIAN_POINT('Ctrl Pts',(0.903949681684066,21.9454122767402,-1.78750548470436));
#10049=CARTESIAN_POINT('Ctrl Pts',(1.38291033277679,22.1537456100734,-1.54529289749877));
#10050=CARTESIAN_POINT('Ctrl Pts',(1.67659613043343,22.3620789434069,-1.09605031831595));
#10051=CARTESIAN_POINT('Ctrl Pts',(1.97028192809003,22.5704122767401,-0.646807739133152));
#10052=CARTESIAN_POINT('Ctrl Pts',(2.,22.7787456100735,-0.110909354270945));
#10053=CARTESIAN_POINT('Ctrl Pts',(2.02971807190997,22.9870789434068,0.42498903059134));
#10054=CARTESIAN_POINT('Ctrl Pts',(1.78750548470433,23.1954122767402,0.903949681684009));
#10055=CARTESIAN_POINT('Ctrl Pts',(1.54529289749872,23.4037456100734,1.38291033277679));
#10056=CARTESIAN_POINT('Ctrl Pts',(1.09605031831593,23.6120789434068,1.6765961304334));
#10057=CARTESIAN_POINT('Ctrl Pts',(0.646807739133168,23.8204122767401,1.97028192809006));
#10058=CARTESIAN_POINT('Ctrl Pts',(0.110909354270907,24.0287456100735,1.99999999999992));
#10059=CARTESIAN_POINT('Ctrl Pts',(-0.424989030591338,24.2370789434068,
2.02971807190996));
#10060=CARTESIAN_POINT('Ctrl Pts',(-0.903949681684066,24.4454122767402,
1.78750548470424));
#10061=CARTESIAN_POINT('Ctrl Pts',(-1.38291033277678,24.6537456100735,1.54529289749864));
#10062=CARTESIAN_POINT('Ctrl Pts',(-1.67659613043341,24.8620789434068,1.09605031831588));
#10063=CARTESIAN_POINT('Ctrl Pts',(-1.97028192809005,25.0704122767401,0.646807739133166));
#10064=CARTESIAN_POINT('Ctrl Pts',(-2.,25.2787456100735,0.110909354270855));
#10065=CARTESIAN_POINT('Ctrl Pts',(-2.02971807190995,25.4870789434068,-0.424989030591369));
#10066=CARTESIAN_POINT('Ctrl Pts',(-1.78750548470433,25.6954122767401,-0.903949681684079));
#10067=CARTESIAN_POINT('Ctrl Pts',(-1.54529289749871,25.9037456100735,-1.3829103327768));
#10068=CARTESIAN_POINT('Ctrl Pts',(-1.09605031831593,26.1120789434068,-1.67659613043345));
#10069=CARTESIAN_POINT('Ctrl Pts',(-0.646807739133152,26.3204122767401,
-1.97028192809011));
#10070=CARTESIAN_POINT('Ctrl Pts',(-0.110909354270907,26.5287456100735,
-2.00000000000004));
#10071=CARTESIAN_POINT('Ctrl Pts',(0.424989030591353,26.7370789434068,-2.02971807190995));
#10072=CARTESIAN_POINT('Ctrl Pts',(0.90394968168408,26.9454122767402,-1.78750548470438));
#10073=CARTESIAN_POINT('Ctrl Pts',(1.38291033277679,27.1537456100734,-1.54529289749872));
#10074=CARTESIAN_POINT('Ctrl Pts',(1.6765961304334,27.3620789434068,-1.09605031831597));
#10075=CARTESIAN_POINT('Ctrl Pts',(1.97028192809005,27.5704122767401,-0.64680773913318));
#10076=CARTESIAN_POINT('Ctrl Pts',(1.99999999999997,27.7787456100735,-0.110909354270911));
#10077=CARTESIAN_POINT('Ctrl Pts',(2.02971807190995,27.9870789434068,0.424989030591333));
#10078=CARTESIAN_POINT('Ctrl Pts',(1.78750548470433,28.1954122767402,0.903949681684037));
#10079=CARTESIAN_POINT('Ctrl Pts',(1.5452928974987,28.4037456100735,1.38291033277679));
#10080=CARTESIAN_POINT('Ctrl Pts',(1.09605031831593,28.6120789434068,1.67659613043337));
#10081=CARTESIAN_POINT('Ctrl Pts',(0.646807739133154,28.8204122767401,1.97028192809002));
#10082=CARTESIAN_POINT('Ctrl Pts',(0.110909354270921,29.0287456100735,1.99999999999997));
#10083=CARTESIAN_POINT('Ctrl Pts',(-0.424989030591338,29.2370789434068,
2.02971807190995));
#10084=CARTESIAN_POINT('Ctrl Pts',(-0.903949681684064,29.4454122767402,
1.78750548470427));
#10085=CARTESIAN_POINT('Ctrl Pts',(-1.38291033277679,29.6537456100735,1.54529289749868));
#10086=CARTESIAN_POINT('Ctrl Pts',(-1.67659613043342,29.8620789434068,1.09605031831586));
#10087=CARTESIAN_POINT('Ctrl Pts',(-1.97028192809005,30.0704122767401,0.646807739133123));
#10088=CARTESIAN_POINT('Ctrl Pts',(-2.,30.2787456100735,0.110909354270834));
#10089=CARTESIAN_POINT('Ctrl Pts',(-2.02971807190995,30.4870789434068,-0.424989030591398));
#10090=CARTESIAN_POINT('Ctrl Pts',(-1.78750548470432,30.6954122767402,-0.903949681684113));
#10091=CARTESIAN_POINT('Ctrl Pts',(-1.54529289749872,30.9037456100735,-1.38291033277676));
#10092=CARTESIAN_POINT('Ctrl Pts',(-1.09605031831593,31.1120789434068,-1.67659613043348));
#10093=CARTESIAN_POINT('Ctrl Pts',(-0.646807739133152,31.3204122767401,
-1.97028192809006));
#10094=CARTESIAN_POINT('Ctrl Pts',(-0.110909354270905,31.5287456100735,
-2.));
#10095=CARTESIAN_POINT('Ctrl Pts',(0.42498903059134,31.7370789434068,-2.02971807190996));
#10096=CARTESIAN_POINT('Ctrl Pts',(0.903949681684054,31.9454122767402,-1.78750548470435));
#10097=CARTESIAN_POINT('Ctrl Pts',(1.38291033277679,32.1537456100735,-1.54529289749877));
#10098=CARTESIAN_POINT('Ctrl Pts',(1.67659613043342,32.3620789434069,-1.09605031831598));
#10099=CARTESIAN_POINT('Ctrl Pts',(1.97028192809005,32.5704122767401,-0.646807739133152));
#10100=CARTESIAN_POINT('Ctrl Pts',(2.,32.7787456100735,-0.110909354270917));
#10101=CARTESIAN_POINT('Ctrl Pts',(2.02971807190995,32.9870789434069,0.424989030591311));
#10102=CARTESIAN_POINT('Ctrl Pts',(1.78750548470433,33.1954122767402,0.903949681684009));
#10103=CARTESIAN_POINT('Ctrl Pts',(1.54529289749872,33.4037456100734,1.38291033277681));
#10104=CARTESIAN_POINT('Ctrl Pts',(1.09605031831593,33.6120789434068,1.67659613043341));
#10105=CARTESIAN_POINT('Ctrl Pts',(0.646807739133154,33.8204122767401,1.97028192809006));
#10106=CARTESIAN_POINT('Ctrl Pts',(0.110909354270907,34.0287456100735,1.99999999999993));
#10107=CARTESIAN_POINT('Ctrl Pts',(-0.424989030591338,34.2370789434068,
2.02971807190994));
#10108=CARTESIAN_POINT('Ctrl Pts',(-0.903949681684066,34.4454122767402,
1.78750548470426));
#10109=CARTESIAN_POINT('Ctrl Pts',(-1.38291033277681,34.6537456100735,1.54529289749869));
#10110=CARTESIAN_POINT('Ctrl Pts',(-1.67659613043341,34.8620789434068,1.0960503183159));
#10111=CARTESIAN_POINT('Ctrl Pts',(-1.97028192809005,35.0704122767402,0.646807739133166));
#10112=CARTESIAN_POINT('Ctrl Pts',(-2.,35.2787456100736,0.110909354270855));
#10113=CARTESIAN_POINT('Ctrl Pts',(-2.02971807190995,35.4870789434068,-0.424989030591383));
#10114=CARTESIAN_POINT('Ctrl Pts',(-1.78750548470433,35.6954122767402,-0.903949681684099));
#10115=CARTESIAN_POINT('Ctrl Pts',(-1.54529289749872,35.9037456100735,-1.38291033277681));
#10116=CARTESIAN_POINT('Ctrl Pts',(-1.09605031831593,36.1120789434069,-1.67659613043344));
#10117=CARTESIAN_POINT('Ctrl Pts',(-0.646807739133139,36.3204122767402,
-1.97028192809006));
#10118=CARTESIAN_POINT('Ctrl Pts',(-0.110909354270907,36.5287456100735,
-2.00000000000004));
#10119=CARTESIAN_POINT('Ctrl Pts',(0.424989030591338,36.7370789434068,-2.02971807190996));
#10120=CARTESIAN_POINT('Ctrl Pts',(0.903949681684066,36.9454122767402,-1.78750548470439));
#10121=CARTESIAN_POINT('Ctrl Pts',(1.38291033277679,37.1537456100734,-1.54529289749872));
#10122=CARTESIAN_POINT('Ctrl Pts',(1.67659613043343,37.3620789434069,-1.09605031831598));
#10123=CARTESIAN_POINT('Ctrl Pts',(1.97028192809006,37.5704122767401,-0.646807739133152));
#10124=CARTESIAN_POINT('Ctrl Pts',(2.,37.7787456100735,-0.110909354270952));
#10125=CARTESIAN_POINT('Ctrl Pts',(2.02971807190997,37.9870789434069,0.424989030591333));
#10126=CARTESIAN_POINT('Ctrl Pts',(1.78750548470433,38.1954122767402,0.903949681684023));
#10127=CARTESIAN_POINT('Ctrl Pts',(1.54529289749872,38.4037456100734,1.3829103327768));
#10128=CARTESIAN_POINT('Ctrl Pts',(1.09605031831595,38.6120789434069,1.67659613043338));
#10129=CARTESIAN_POINT('Ctrl Pts',(0.646807739133154,38.8204122767402,1.97028192809006));
#10130=CARTESIAN_POINT('Ctrl Pts',(0.110909354270921,39.0287456100735,1.99999999999997));
#10131=CARTESIAN_POINT('Ctrl Pts',(-0.424989030591324,39.2370789434069,
2.02971807190996));
#10132=CARTESIAN_POINT('Ctrl Pts',(-0.903949681684052,39.4454122767402,
1.78750548470429));
#10133=CARTESIAN_POINT('Ctrl Pts',(-1.38291033277679,39.6537456100735,1.54529289749867));
#10134=CARTESIAN_POINT('Ctrl Pts',(-1.67659613043342,39.8620789434069,1.09605031831587));
#10135=CARTESIAN_POINT('Ctrl Pts',(-1.97028192809005,40.0704122767402,0.646807739133166));
#10136=CARTESIAN_POINT('Ctrl Pts',(-2.,40.2787456100735,0.110909354270834));
#10137=CARTESIAN_POINT('Ctrl Pts',(-1.40000000000002,0.278745610073447,
0.110909354270819));
#10138=CARTESIAN_POINT('Ctrl Pts',(-1.42971807190993,0.487078943406762,
-0.264219515132761));
#10139=CARTESIAN_POINT('Ctrl Pts',(-1.26789024243367,0.695412276740075,
-0.603949681684109));
#10140=CARTESIAN_POINT('Ctrl Pts',(-1.10606241295736,0.903745610073446,
-0.943679848235563));
#10141=CARTESIAN_POINT('Ctrl Pts',(-0.796050318315929,1.11207894340677,
-1.1569808881628));
#10142=CARTESIAN_POINT('Ctrl Pts',(-0.486038223674453,1.3204122767401,-1.37028192809014));
#10143=CARTESIAN_POINT('Ctrl Pts',(-0.110909354270902,1.52874561007343,
-1.40000000000009));
#10144=CARTESIAN_POINT('Ctrl Pts',(0.26421951513267,1.73707894340676,-1.42971807191003));
#10145=CARTESIAN_POINT('Ctrl Pts',(0.60394968168407,1.9454122767401,-1.26789024243367));
#10146=CARTESIAN_POINT('Ctrl Pts',(0.943679848235471,2.15374561007345,-1.10606241295738));
#10147=CARTESIAN_POINT('Ctrl Pts',(1.15698088816274,2.36207894340676,-0.796050318316012));
#10148=CARTESIAN_POINT('Ctrl Pts',(1.37028192809006,2.5704122767401,-0.486038223674555));
#10149=CARTESIAN_POINT('Ctrl Pts',(1.39999999999998,2.77874561007344,-0.110909354270902));
#10150=CARTESIAN_POINT('Ctrl Pts',(1.42971807190994,2.98707894340678,0.264219515132648));
#10151=CARTESIAN_POINT('Ctrl Pts',(1.26789024243366,3.19541227674007,0.60394968168399));
#10152=CARTESIAN_POINT('Ctrl Pts',(1.10606241295741,3.40374561007344,0.943679848235385));
#10153=CARTESIAN_POINT('Ctrl Pts',(0.796050318315931,3.61207894340678,1.15698088816276));
#10154=CARTESIAN_POINT('Ctrl Pts',(0.486038223674496,3.82041227674011,1.37028192808997));
#10155=CARTESIAN_POINT('Ctrl Pts',(0.110909354270899,4.02874561007344,1.4));
#10156=CARTESIAN_POINT('Ctrl Pts',(-0.264219515132648,4.23707894340677,
1.42971807190986));
#10157=CARTESIAN_POINT('Ctrl Pts',(-0.603949681684091,4.44541227674011,
1.2678902424336));
#10158=CARTESIAN_POINT('Ctrl Pts',(-0.943679848235468,4.65374561007345,
1.1060624129573));
#10159=CARTESIAN_POINT('Ctrl Pts',(-1.15698088816278,4.86207894340679,0.796050318315845));
#10160=CARTESIAN_POINT('Ctrl Pts',(-1.37028192809003,5.07041227674011,0.486038223674474));
#10161=CARTESIAN_POINT('Ctrl Pts',(-1.40000000000002,5.27874561007345,0.110909354270819));
#10162=CARTESIAN_POINT('Ctrl Pts',(-1.42971807190992,5.4870789434068,-0.264219515132837));
#10163=CARTESIAN_POINT('Ctrl Pts',(-1.26789024243366,5.69541227674011,-0.603949681684078));
#10164=CARTESIAN_POINT('Ctrl Pts',(-1.10606241295738,5.90374561007345,-0.943679848235563));
#10165=CARTESIAN_POINT('Ctrl Pts',(-0.79605031831595,6.11207894340678,-1.15698088816284));
#10166=CARTESIAN_POINT('Ctrl Pts',(-0.486038223674474,6.32041227674012,
-1.37028192809014));
#10167=CARTESIAN_POINT('Ctrl Pts',(-0.110909354270923,6.52874561007347,
-1.40000000000009));
#10168=CARTESIAN_POINT('Ctrl Pts',(0.264219515132672,6.7370789434068,-1.42971807191003));
#10169=CARTESIAN_POINT('Ctrl Pts',(0.60394968168407,6.94541227674011,-1.26789024243367));
#10170=CARTESIAN_POINT('Ctrl Pts',(0.943679848235474,7.15374561007344,-1.10606241295738));
#10171=CARTESIAN_POINT('Ctrl Pts',(1.15698088816276,7.36207894340676,-0.796050318316012));
#10172=CARTESIAN_POINT('Ctrl Pts',(1.37028192809008,7.57041227674013,-0.486038223674566));
#10173=CARTESIAN_POINT('Ctrl Pts',(1.4,7.77874561007344,-0.110909354270902));
#10174=CARTESIAN_POINT('Ctrl Pts',(1.42971807190995,7.98707894340678,0.264219515132605));
#10175=CARTESIAN_POINT('Ctrl Pts',(1.26789024243366,8.19541227674011,0.603949681683985));
#10176=CARTESIAN_POINT('Ctrl Pts',(1.10606241295739,8.40374561007346,0.943679848235385));
#10177=CARTESIAN_POINT('Ctrl Pts',(0.796050318315911,8.6120789434068,1.15698088816276));
#10178=CARTESIAN_POINT('Ctrl Pts',(0.486038223674474,8.82041227674011,1.37028192809001));
#10179=CARTESIAN_POINT('Ctrl Pts',(0.110909354270881,9.02874561007344,1.4));
#10180=CARTESIAN_POINT('Ctrl Pts',(-0.264219515132648,9.23707894340678,
1.42971807190988));
#10181=CARTESIAN_POINT('Ctrl Pts',(-0.603949681684091,9.44541227674012,
1.26789024243366));
#10182=CARTESIAN_POINT('Ctrl Pts',(-0.943679848235471,9.65374561007344,
1.1060624129573));
#10183=CARTESIAN_POINT('Ctrl Pts',(-1.15698088816276,9.86207894340679,0.796050318315845));
#10184=CARTESIAN_POINT('Ctrl Pts',(-1.37028192809006,10.0704122767401,0.486038223674393));
#10185=CARTESIAN_POINT('Ctrl Pts',(-1.40000000000002,10.2787456100734,0.110909354270819));
#10186=CARTESIAN_POINT('Ctrl Pts',(-1.42971807190993,10.4870789434068,-0.264219515132756));
#10187=CARTESIAN_POINT('Ctrl Pts',(-1.26789024243369,10.6954122767401,-0.60394968168412));
#10188=CARTESIAN_POINT('Ctrl Pts',(-1.10606241295736,10.9037456100735,-0.94367984823553));
#10189=CARTESIAN_POINT('Ctrl Pts',(-0.79605031831595,11.1120789434068,-1.15698088816285));
#10190=CARTESIAN_POINT('Ctrl Pts',(-0.486038223674453,11.3204122767401,
-1.37028192809014));
#10191=CARTESIAN_POINT('Ctrl Pts',(-0.110909354270923,11.5287456100735,
-1.40000000000009));
#10192=CARTESIAN_POINT('Ctrl Pts',(0.264219515132691,11.7370789434068,-1.42971807191005));
#10193=CARTESIAN_POINT('Ctrl Pts',(0.60394968168405,11.9454122767401,-1.26789024243367));
#10194=CARTESIAN_POINT('Ctrl Pts',(0.943679848235492,12.1537456100735,-1.10606241295747));
#10195=CARTESIAN_POINT('Ctrl Pts',(1.15698088816276,12.3620789434068,-0.796050318316012));
#10196=CARTESIAN_POINT('Ctrl Pts',(1.37028192809006,12.5704122767401,-0.48603822367456));
#10197=CARTESIAN_POINT('Ctrl Pts',(1.4,12.7787456100735,-0.110909354270902));
#10198=CARTESIAN_POINT('Ctrl Pts',(1.42971807190997,12.9870789434068,0.264219515132578));
#10199=CARTESIAN_POINT('Ctrl Pts',(1.26789024243366,13.1954122767402,0.603949681683979));
#10200=CARTESIAN_POINT('Ctrl Pts',(1.10606241295738,13.4037456100734,0.943679848235428));
#10201=CARTESIAN_POINT('Ctrl Pts',(0.796050318315911,13.6120789434068,1.15698088816276));
#10202=CARTESIAN_POINT('Ctrl Pts',(0.486038223674477,13.8204122767401,1.37028192809001));
#10203=CARTESIAN_POINT('Ctrl Pts',(0.110909354270902,14.0287456100735,1.4));
#10204=CARTESIAN_POINT('Ctrl Pts',(-0.264219515132648,14.2370789434068,
1.42971807190986));
#10205=CARTESIAN_POINT('Ctrl Pts',(-0.603949681684091,14.4454122767401,
1.26789024243366));
#10206=CARTESIAN_POINT('Ctrl Pts',(-0.943679848235471,14.6537456100735,
1.10606241295732));
#10207=CARTESIAN_POINT('Ctrl Pts',(-1.15698088816278,14.8620789434068,0.796050318315845));
#10208=CARTESIAN_POINT('Ctrl Pts',(-1.37028192809005,15.0704122767401,0.48603822367442));
#10209=CARTESIAN_POINT('Ctrl Pts',(-1.4,15.2787456100735,0.110909354270819));
#10210=CARTESIAN_POINT('Ctrl Pts',(-1.42971807190992,15.4870789434068,-0.264219515132718));
#10211=CARTESIAN_POINT('Ctrl Pts',(-1.26789024243366,15.6954122767401,-0.603949681684167));
#10212=CARTESIAN_POINT('Ctrl Pts',(-1.10606241295736,15.9037456100735,-0.943679848235573));
#10213=CARTESIAN_POINT('Ctrl Pts',(-0.796050318315929,16.1120789434068,
-1.15698088816286));
#10214=CARTESIAN_POINT('Ctrl Pts',(-0.486038223674453,16.3204122767402,
-1.37028192809016));
#10215=CARTESIAN_POINT('Ctrl Pts',(-0.110909354270902,16.5287456100735,
-1.40000000000009));
#10216=CARTESIAN_POINT('Ctrl Pts',(0.264219515132672,16.7370789434068,-1.42971807191007));
#10217=CARTESIAN_POINT('Ctrl Pts',(0.60394968168407,16.9454122767402,-1.26789024243367));
#10218=CARTESIAN_POINT('Ctrl Pts',(0.943679848235471,17.1537456100735,-1.10606241295741));
#10219=CARTESIAN_POINT('Ctrl Pts',(1.15698088816274,17.3620789434068,-0.796050318316007));
#10220=CARTESIAN_POINT('Ctrl Pts',(1.37028192809005,17.5704122767402,-0.486038223674528));
#10221=CARTESIAN_POINT('Ctrl Pts',(1.39999999999998,17.7787456100735,-0.110909354270907));
#10222=CARTESIAN_POINT('Ctrl Pts',(1.42971807190994,17.9870789434068,0.2642195151326));
#10223=CARTESIAN_POINT('Ctrl Pts',(1.26789024243364,18.1954122767402,0.603949681683979));
#10224=CARTESIAN_POINT('Ctrl Pts',(1.10606241295739,18.4037456100735,0.943679848235406));
#10225=CARTESIAN_POINT('Ctrl Pts',(0.796050318315929,18.6120789434068,1.15698088816276));
#10226=CARTESIAN_POINT('Ctrl Pts',(0.486038223674496,18.8204122767402,1.37028192808999));
#10227=CARTESIAN_POINT('Ctrl Pts',(0.110909354270902,19.0287456100735,1.39999999999996));
#10228=CARTESIAN_POINT('Ctrl Pts',(-0.26421951513267,19.2370789434068,1.42971807190988));
#10229=CARTESIAN_POINT('Ctrl Pts',(-0.60394968168407,19.4454122767402,1.26789024243363));
#10230=CARTESIAN_POINT('Ctrl Pts',(-0.943679848235452,19.6537456100735,
1.1060624129573));
#10231=CARTESIAN_POINT('Ctrl Pts',(-1.15698088816278,19.8620789434068,0.796050318315845));
#10232=CARTESIAN_POINT('Ctrl Pts',(-1.37028192809005,20.0704122767402,0.486038223674393));
#10233=CARTESIAN_POINT('Ctrl Pts',(-1.4,20.2787456100735,0.110909354270813));
#10234=CARTESIAN_POINT('Ctrl Pts',(-1.42971807190994,20.4870789434068,-0.26421951513274));
#10235=CARTESIAN_POINT('Ctrl Pts',(-1.26789024243366,20.6954122767402,-0.603949681684167));
#10236=CARTESIAN_POINT('Ctrl Pts',(-1.10606241295736,20.9037456100735,-0.943679848235573));
#10237=CARTESIAN_POINT('Ctrl Pts',(-0.79605031831595,21.1120789434068,-1.15698088816285));
#10238=CARTESIAN_POINT('Ctrl Pts',(-0.486038223674453,21.3204122767402,
-1.37028192809015));
#10239=CARTESIAN_POINT('Ctrl Pts',(-0.110909354270923,21.5287456100735,
-1.4000000000001));
#10240=CARTESIAN_POINT('Ctrl Pts',(0.264219515132691,21.7370789434068,-1.42971807191004));
#10241=CARTESIAN_POINT('Ctrl Pts',(0.60394968168407,21.9454122767402,-1.26789024243367));
#10242=CARTESIAN_POINT('Ctrl Pts',(0.943679848235474,22.1537456100735,-1.10606241295747));
#10243=CARTESIAN_POINT('Ctrl Pts',(1.15698088816276,22.3620789434068,-0.796050318316001));
#10244=CARTESIAN_POINT('Ctrl Pts',(1.37028192809006,22.5704122767402,-0.486038223674555));
#10245=CARTESIAN_POINT('Ctrl Pts',(1.4,22.7787456100735,-0.110909354270928));
#10246=CARTESIAN_POINT('Ctrl Pts',(1.42971807190997,22.9870789434068,0.264219515132573));
#10247=CARTESIAN_POINT('Ctrl Pts',(1.26789024243366,23.1954122767402,0.603949681684057));
#10248=CARTESIAN_POINT('Ctrl Pts',(1.10606241295738,23.4037456100735,0.943679848235433));
#10249=CARTESIAN_POINT('Ctrl Pts',(0.796050318315926,23.6120789434068,1.15698088816273));
#10250=CARTESIAN_POINT('Ctrl Pts',(0.486038223674474,23.8204122767402,1.37028192809002));
#10251=CARTESIAN_POINT('Ctrl Pts',(0.110909354270881,24.0287456100735,1.39999999999998));
#10252=CARTESIAN_POINT('Ctrl Pts',(-0.264219515132651,24.2370789434069,
1.42971807190985));
#10253=CARTESIAN_POINT('Ctrl Pts',(-0.603949681684091,24.4454122767401,
1.2678902424336));
#10254=CARTESIAN_POINT('Ctrl Pts',(-0.943679848235471,24.6537456100735,
1.10606241295733));
#10255=CARTESIAN_POINT('Ctrl Pts',(-1.15698088816276,24.8620789434068,0.796050318315887));
#10256=CARTESIAN_POINT('Ctrl Pts',(-1.37028192809005,25.0704122767401,0.486038223674404));
#10257=CARTESIAN_POINT('Ctrl Pts',(-1.4,25.2787456100735,0.110909354270813));
#10258=CARTESIAN_POINT('Ctrl Pts',(-1.42971807190994,25.4870789434068,-0.264219515132734));
#10259=CARTESIAN_POINT('Ctrl Pts',(-1.26789024243369,25.6954122767402,-0.603949681684162));
#10260=CARTESIAN_POINT('Ctrl Pts',(-1.10606241295738,25.9037456100735,-0.943679848235541));
#10261=CARTESIAN_POINT('Ctrl Pts',(-0.79605031831595,26.1120789434068,-1.15698088816286));
#10262=CARTESIAN_POINT('Ctrl Pts',(-0.486038223674453,26.3204122767402,
-1.37028192809015));
#10263=CARTESIAN_POINT('Ctrl Pts',(-0.110909354270923,26.5287456100735,
-1.4000000000001));
#10264=CARTESIAN_POINT('Ctrl Pts',(0.264219515132694,26.7370789434069,-1.42971807191004));
#10265=CARTESIAN_POINT('Ctrl Pts',(0.60394968168405,26.9454122767402,-1.26789024243367));
#10266=CARTESIAN_POINT('Ctrl Pts',(0.943679848235492,27.1537456100735,-1.10606241295747));
#10267=CARTESIAN_POINT('Ctrl Pts',(1.15698088816274,27.3620789434069,-0.796050318316001));
#10268=CARTESIAN_POINT('Ctrl Pts',(1.37028192809008,27.5704122767402,-0.486038223674528));
#10269=CARTESIAN_POINT('Ctrl Pts',(1.39999999999998,27.7787456100735,-0.110909354270917));
#10270=CARTESIAN_POINT('Ctrl Pts',(1.42971807190997,27.9870789434068,0.264219515132594));
#10271=CARTESIAN_POINT('Ctrl Pts',(1.26789024243366,28.1954122767402,0.603949681684047));
#10272=CARTESIAN_POINT('Ctrl Pts',(1.10606241295738,28.4037456100735,0.943679848235406));
#10273=CARTESIAN_POINT('Ctrl Pts',(0.796050318315908,28.6120789434068,1.15698088816274));
#10274=CARTESIAN_POINT('Ctrl Pts',(0.486038223674496,28.8204122767402,1.37028192809));
#10275=CARTESIAN_POINT('Ctrl Pts',(0.110909354270902,29.0287456100735,1.39999999999997));
#10276=CARTESIAN_POINT('Ctrl Pts',(-0.26421951513267,29.2370789434068,1.42971807190989));
#10277=CARTESIAN_POINT('Ctrl Pts',(-0.603949681684091,29.4454122767402,
1.26789024243359));
#10278=CARTESIAN_POINT('Ctrl Pts',(-0.943679848235452,29.6537456100735,
1.10606241295731));
#10279=CARTESIAN_POINT('Ctrl Pts',(-1.15698088816278,29.8620789434069,0.796050318315892));
#10280=CARTESIAN_POINT('Ctrl Pts',(-1.37028192809005,30.0704122767402,0.486038223674393));
#10281=CARTESIAN_POINT('Ctrl Pts',(-1.4,30.2787456100735,0.11090935427086));
#10282=CARTESIAN_POINT('Ctrl Pts',(-1.42971807190994,30.4870789434069,-0.26421951513274));
#10283=CARTESIAN_POINT('Ctrl Pts',(-1.26789024243366,30.6954122767402,-0.603949681684162));
#10284=CARTESIAN_POINT('Ctrl Pts',(-1.10606241295736,30.9037456100735,-0.943679848235563));
#10285=CARTESIAN_POINT('Ctrl Pts',(-0.79605031831595,31.1120789434068,-1.15698088816285));
#10286=CARTESIAN_POINT('Ctrl Pts',(-0.486038223674471,31.3204122767402,
-1.37028192809016));
#10287=CARTESIAN_POINT('Ctrl Pts',(-0.110909354270923,31.5287456100735,
-1.4000000000001));
#10288=CARTESIAN_POINT('Ctrl Pts',(0.264219515132691,31.7370789434069,-1.42971807191));
#10289=CARTESIAN_POINT('Ctrl Pts',(0.60394968168407,31.9454122767402,-1.26789024243368));
#10290=CARTESIAN_POINT('Ctrl Pts',(0.943679848235474,32.1537456100735,-1.10606241295744));
#10291=CARTESIAN_POINT('Ctrl Pts',(1.15698088816274,32.3620789434069,-0.796050318315981));
#10292=CARTESIAN_POINT('Ctrl Pts',(1.37028192809005,32.5704122767402,-0.48603822367455));
#10293=CARTESIAN_POINT('Ctrl Pts',(1.4,32.7787456100735,-0.110909354270917));
#10294=CARTESIAN_POINT('Ctrl Pts',(1.42971807190994,32.9870789434069,0.264219515132578));
#10295=CARTESIAN_POINT('Ctrl Pts',(1.26789024243364,33.1954122767402,0.603949681684047));
#10296=CARTESIAN_POINT('Ctrl Pts',(1.10606241295741,33.4037456100735,0.943679848235428));
#10297=CARTESIAN_POINT('Ctrl Pts',(0.796050318315929,33.6120789434069,1.15698088816274));
#10298=CARTESIAN_POINT('Ctrl Pts',(0.486038223674496,33.8204122767402,1.37028192809002));
#10299=CARTESIAN_POINT('Ctrl Pts',(0.110909354270881,34.0287456100735,1.39999999999998));
#10300=CARTESIAN_POINT('Ctrl Pts',(-0.26421951513267,34.2370789434069,1.42971807190985));
#10301=CARTESIAN_POINT('Ctrl Pts',(-0.603949681684091,34.4454122767402,
1.26789024243359));
#10302=CARTESIAN_POINT('Ctrl Pts',(-0.943679848235449,34.6537456100735,
1.10606241295733));
#10303=CARTESIAN_POINT('Ctrl Pts',(-1.15698088816278,34.8620789434069,0.796050318315903));
#10304=CARTESIAN_POINT('Ctrl Pts',(-1.37028192809003,35.0704122767402,0.486038223674404));
#10305=CARTESIAN_POINT('Ctrl Pts',(-1.4,35.2787456100735,0.11090935427086));
#10306=CARTESIAN_POINT('Ctrl Pts',(-1.42971807190994,35.4870789434069,-0.264219515132756));
#10307=CARTESIAN_POINT('Ctrl Pts',(-1.26789024243369,35.6954122767402,-0.603949681684089));
#10308=CARTESIAN_POINT('Ctrl Pts',(-1.10606241295738,35.9037456100736,-0.943679848235563));
#10309=CARTESIAN_POINT('Ctrl Pts',(-0.79605031831595,36.1120789434069,-1.15698088816278));
#10310=CARTESIAN_POINT('Ctrl Pts',(-0.486038223674474,36.3204122767402,
-1.37028192809014));
#10311=CARTESIAN_POINT('Ctrl Pts',(-0.11090935427092,36.5287456100735,-1.40000000000009));
#10312=CARTESIAN_POINT('Ctrl Pts',(0.264219515132672,36.7370789434069,-1.42971807191003));
#10313=CARTESIAN_POINT('Ctrl Pts',(0.60394968168405,36.9454122767402,-1.2678902424337));
#10314=CARTESIAN_POINT('Ctrl Pts',(0.943679848235492,37.1537456100735,-1.10606241295747));
#10315=CARTESIAN_POINT('Ctrl Pts',(1.15698088816274,37.3620789434068,-0.796050318315981));
#10316=CARTESIAN_POINT('Ctrl Pts',(1.37028192809008,37.5704122767402,-0.486038223674555));
#10317=CARTESIAN_POINT('Ctrl Pts',(1.4,37.7787456100735,-0.110909354270923));
#10318=CARTESIAN_POINT('Ctrl Pts',(1.42971807190994,37.9870789434069,0.264219515132605));
#10319=CARTESIAN_POINT('Ctrl Pts',(1.26789024243366,38.1954122767402,0.603949681684011));
#10320=CARTESIAN_POINT('Ctrl Pts',(1.10606241295738,38.4037456100735,0.943679848235417));
#10321=CARTESIAN_POINT('Ctrl Pts',(0.796050318315929,38.6120789434069,1.15698088816273));
#10322=CARTESIAN_POINT('Ctrl Pts',(0.486038223674474,38.8204122767402,1.37028192808999));
#10323=CARTESIAN_POINT('Ctrl Pts',(0.110909354270881,39.0287456100735,1.39999999999998));
#10324=CARTESIAN_POINT('Ctrl Pts',(-0.264219515132648,39.2370789434069,
1.42971807190988));
#10325=CARTESIAN_POINT('Ctrl Pts',(-0.603949681684073,39.4454122767402,
1.26789024243359));
#10326=CARTESIAN_POINT('Ctrl Pts',(-0.943679848235474,39.6537456100736,
1.10606241295731));
#10327=CARTESIAN_POINT('Ctrl Pts',(-1.15698088816278,39.8620789434069,0.796050318315897));
#10328=CARTESIAN_POINT('Ctrl Pts',(-1.37028192809005,40.0704122767402,0.486038223674399));
#10329=CARTESIAN_POINT('Ctrl Pts',(-1.4,40.2787456100735,0.11090935427086));
#10330=CARTESIAN_POINT('Ctrl Pts',(-1.4,-0.278745610073483,-0.110909354270949));
#10331=CARTESIAN_POINT('Ctrl Pts',(-1.37028192809006,-0.0704122767401418,
-0.486038223674447));
#10332=CARTESIAN_POINT('Ctrl Pts',(-1.1569808881628,0.137921056593191,-0.796050318316017));
#10333=CARTESIAN_POINT('Ctrl Pts',(-0.943679848235495,0.346254389926559,
-1.10606241295736));
#10334=CARTESIAN_POINT('Ctrl Pts',(-0.60394968168412,0.554587723259871,
-1.26789024243366));
#10335=CARTESIAN_POINT('Ctrl Pts',(-0.264219515132702,0.762921056593206,
-1.42971807191002));
#10336=CARTESIAN_POINT('Ctrl Pts',(0.11090935427085,0.971254389926519,-1.39999999999999));
#10337=CARTESIAN_POINT('Ctrl Pts',(0.486038223674463,1.17958772325989,-1.37028192809015));
#10338=CARTESIAN_POINT('Ctrl Pts',(0.7960503183159,1.3879210565932,-1.15698088816281));
#10339=CARTESIAN_POINT('Ctrl Pts',(1.10606241295738,1.59625438992658,-0.943679848235584));
#10340=CARTESIAN_POINT('Ctrl Pts',(1.26789024243364,1.80458772325987,-0.603949681684177));
#10341=CARTESIAN_POINT('Ctrl Pts',(1.42971807190996,2.01292105659321,-0.264219515132788));
#10342=CARTESIAN_POINT('Ctrl Pts',(1.39999999999998,2.22125438992654,0.110909354270787));
#10343=CARTESIAN_POINT('Ctrl Pts',(1.37028192809009,2.42958772325987,0.486038223674361));
#10344=CARTESIAN_POINT('Ctrl Pts',(1.15698088816276,2.63792105659322,0.796050318315897));
#10345=CARTESIAN_POINT('Ctrl Pts',(0.943679848235517,2.84625438992656,1.10606241295735));
#10346=CARTESIAN_POINT('Ctrl Pts',(0.603949681684099,3.05458772325989,1.26789024243365));
#10347=CARTESIAN_POINT('Ctrl Pts',(0.264219515132705,3.26292105659324,1.42971807190985));
#10348=CARTESIAN_POINT('Ctrl Pts',(-0.110909354270889,3.47125438992654,
1.39999999999992));
#10349=CARTESIAN_POINT('Ctrl Pts',(-0.48603822367442,3.67958772325988,1.37028192808998));
#10350=CARTESIAN_POINT('Ctrl Pts',(-0.796050318315921,3.8879210565932,1.15698088816272));
#10351=CARTESIAN_POINT('Ctrl Pts',(-1.10606241295734,4.09625438992655,0.943679848235406));
#10352=CARTESIAN_POINT('Ctrl Pts',(-1.26789024243365,4.30458772325989,0.603949681684094));
#10353=CARTESIAN_POINT('Ctrl Pts',(-1.42971807190994,4.51292105659323,0.2642195151326));
#10354=CARTESIAN_POINT('Ctrl Pts',(-1.4,4.72125438992655,-0.110909354270949));
#10355=CARTESIAN_POINT('Ctrl Pts',(-1.37028192809004,4.9295877232599,-0.486038223674442));
#10356=CARTESIAN_POINT('Ctrl Pts',(-1.15698088816278,5.13792105659321,-0.796050318315991));
#10357=CARTESIAN_POINT('Ctrl Pts',(-0.943679848235495,5.34625438992658,
-1.10606241295745));
#10358=CARTESIAN_POINT('Ctrl Pts',(-0.603949681684099,5.55458772325993,
-1.26789024243366));
#10359=CARTESIAN_POINT('Ctrl Pts',(-0.264219515132702,5.76292105659326,
-1.42971807190998));
#10360=CARTESIAN_POINT('Ctrl Pts',(0.110909354270868,5.97125438992656,-1.40000000000003));
#10361=CARTESIAN_POINT('Ctrl Pts',(0.486038223674442,6.17958772325989,-1.37028192809015));
#10362=CARTESIAN_POINT('Ctrl Pts',(0.796050318315879,6.38792105659323,-1.15698088816278));
#10363=CARTESIAN_POINT('Ctrl Pts',(1.10606241295736,6.59625438992658,-0.943679848235606));
#10364=CARTESIAN_POINT('Ctrl Pts',(1.26789024243365,6.80458772325986,-0.603949681684177));
#10365=CARTESIAN_POINT('Ctrl Pts',(1.42971807190994,7.01292105659325,-0.264219515132794));
#10366=CARTESIAN_POINT('Ctrl Pts',(1.4,7.22125438992654,0.110909354270824));
#10367=CARTESIAN_POINT('Ctrl Pts',(1.37028192809007,7.42958772325991,0.486038223674361));
#10368=CARTESIAN_POINT('Ctrl Pts',(1.15698088816276,7.63792105659323,0.796050318315897));
#10369=CARTESIAN_POINT('Ctrl Pts',(0.943679848235498,7.84625438992655,1.10606241295728));
#10370=CARTESIAN_POINT('Ctrl Pts',(0.603949681684078,8.05458772325989,1.26789024243365));
#10371=CARTESIAN_POINT('Ctrl Pts',(0.264219515132724,8.26292105659323,1.42971807190989));
#10372=CARTESIAN_POINT('Ctrl Pts',(-0.110909354270889,8.47125438992655,
1.39999999999992));
#10373=CARTESIAN_POINT('Ctrl Pts',(-0.486038223674439,8.67958772325992,
1.37028192808998));
#10374=CARTESIAN_POINT('Ctrl Pts',(-0.796050318315921,8.88792105659323,
1.15698088816273));
#10375=CARTESIAN_POINT('Ctrl Pts',(-1.10606241295736,9.09625438992657,0.94367984823539));
#10376=CARTESIAN_POINT('Ctrl Pts',(-1.26789024243365,9.3045877232599,0.603949681684094));
#10377=CARTESIAN_POINT('Ctrl Pts',(-1.42971807190994,9.51292105659322,0.264219515132616));
#10378=CARTESIAN_POINT('Ctrl Pts',(-1.4,9.72125438992658,-0.110909354270954));
#10379=CARTESIAN_POINT('Ctrl Pts',(-1.37028192809006,9.92958772325988,-0.486038223674523));
#10380=CARTESIAN_POINT('Ctrl Pts',(-1.1569808881628,10.1379210565933,-0.796050318315991));
#10381=CARTESIAN_POINT('Ctrl Pts',(-0.943679848235474,10.3462543899266,
-1.10606241295745));
#10382=CARTESIAN_POINT('Ctrl Pts',(-0.60394968168412,10.5545877232599,-1.26789024243366));
#10383=CARTESIAN_POINT('Ctrl Pts',(-0.264219515132683,10.7629210565932,
-1.42971807191006));
#10384=CARTESIAN_POINT('Ctrl Pts',(0.110909354270847,10.9712543899266,-1.40000000000007));
#10385=CARTESIAN_POINT('Ctrl Pts',(0.486038223674463,11.1795877232599,-1.37028192809018));
#10386=CARTESIAN_POINT('Ctrl Pts',(0.7960503183159,11.3879210565933,-1.15698088816279));
#10387=CARTESIAN_POINT('Ctrl Pts',(1.10606241295736,11.5962543899266,-0.943679848235595));
#10388=CARTESIAN_POINT('Ctrl Pts',(1.26789024243365,11.8045877232599,-0.603949681684188));
#10389=CARTESIAN_POINT('Ctrl Pts',(1.42971807190994,12.0129210565932,-0.264219515132707));
#10390=CARTESIAN_POINT('Ctrl Pts',(1.4,12.2212543899266,0.110909354270855));
#10391=CARTESIAN_POINT('Ctrl Pts',(1.37028192809006,12.4295877232599,0.486038223674382));
#10392=CARTESIAN_POINT('Ctrl Pts',(1.15698088816276,12.6379210565932,0.796050318315897));
#10393=CARTESIAN_POINT('Ctrl Pts',(0.943679848235517,12.8462543899266,1.10606241295731));
#10394=CARTESIAN_POINT('Ctrl Pts',(0.603949681684099,13.0545877232599,1.26789024243365));
#10395=CARTESIAN_POINT('Ctrl Pts',(0.264219515132705,13.2629210565933,1.42971807190989));
#10396=CARTESIAN_POINT('Ctrl Pts',(-0.110909354270889,13.4712543899266,
1.39999999999992));
#10397=CARTESIAN_POINT('Ctrl Pts',(-0.48603822367442,13.6795877232599,1.37028192808998));
#10398=CARTESIAN_POINT('Ctrl Pts',(-0.7960503183159,13.8879210565933,1.15698088816275));
#10399=CARTESIAN_POINT('Ctrl Pts',(-1.10606241295736,14.0962543899266,0.943679848235428));
#10400=CARTESIAN_POINT('Ctrl Pts',(-1.26789024243365,14.3045877232599,0.603949681684078));
#10401=CARTESIAN_POINT('Ctrl Pts',(-1.42971807190992,14.5129210565933,0.264219515132632));
#10402=CARTESIAN_POINT('Ctrl Pts',(-1.40000000000002,14.7212543899266,-0.110909354270954));
#10403=CARTESIAN_POINT('Ctrl Pts',(-1.37028192809007,14.9295877232599,-0.486038223674463));
#10404=CARTESIAN_POINT('Ctrl Pts',(-1.15698088816278,15.1379210565933,-0.796050318315991));
#10405=CARTESIAN_POINT('Ctrl Pts',(-0.943679848235495,15.3462543899266,
-1.10606241295744));
#10406=CARTESIAN_POINT('Ctrl Pts',(-0.60394968168412,15.55458772326,-1.26789024243366));
#10407=CARTESIAN_POINT('Ctrl Pts',(-0.264219515132702,15.7629210565933,
-1.42971807191003));
#10408=CARTESIAN_POINT('Ctrl Pts',(0.110909354270868,15.9712543899266,-1.40000000000008));
#10409=CARTESIAN_POINT('Ctrl Pts',(0.486038223674463,16.1795877232599,-1.37028192809016));
#10410=CARTESIAN_POINT('Ctrl Pts',(0.796050318315879,16.3879210565933,-1.15698088816279));
#10411=CARTESIAN_POINT('Ctrl Pts',(1.10606241295736,16.5962543899266,-0.94367984823559));
#10412=CARTESIAN_POINT('Ctrl Pts',(1.26789024243365,16.8045877232599,-0.603949681684188));
#10413=CARTESIAN_POINT('Ctrl Pts',(1.42971807190996,17.0129210565933,-0.264219515132783));
#10414=CARTESIAN_POINT('Ctrl Pts',(1.39999999999998,17.2212543899266,0.11090935427085));
#10415=CARTESIAN_POINT('Ctrl Pts',(1.37028192809007,17.4295877232599,0.486038223674382));
#10416=CARTESIAN_POINT('Ctrl Pts',(1.15698088816276,17.6379210565933,0.796050318315892));
#10417=CARTESIAN_POINT('Ctrl Pts',(0.943679848235517,17.8462543899266,1.10606241295728));
#10418=CARTESIAN_POINT('Ctrl Pts',(0.603949681684099,18.0545877232599,1.26789024243363));
#10419=CARTESIAN_POINT('Ctrl Pts',(0.264219515132724,18.2629210565933,1.42971807190987));
#10420=CARTESIAN_POINT('Ctrl Pts',(-0.110909354270889,18.4712543899266,
1.39999999999997));
#10421=CARTESIAN_POINT('Ctrl Pts',(-0.48603822367442,18.6795877232599,1.37028192808996));
#10422=CARTESIAN_POINT('Ctrl Pts',(-0.796050318315921,18.8879210565933,
1.15698088816276));
#10423=CARTESIAN_POINT('Ctrl Pts',(-1.10606241295736,19.0962543899266,0.943679848235417));
#10424=CARTESIAN_POINT('Ctrl Pts',(-1.26789024243365,19.3045877232599,0.603949681684037));
#10425=CARTESIAN_POINT('Ctrl Pts',(-1.42971807190994,19.5129210565933,0.264219515132616));
#10426=CARTESIAN_POINT('Ctrl Pts',(-1.4,19.7212543899266,-0.110909354270954));
#10427=CARTESIAN_POINT('Ctrl Pts',(-1.37028192809006,19.9295877232599,-0.486038223674496));
#10428=CARTESIAN_POINT('Ctrl Pts',(-1.1569808881628,20.1379210565933,-0.796050318315996));
#10429=CARTESIAN_POINT('Ctrl Pts',(-0.943679848235474,20.3462543899266,
-1.10606241295739));
#10430=CARTESIAN_POINT('Ctrl Pts',(-0.603949681684099,20.5545877232599,
-1.26789024243366));
#10431=CARTESIAN_POINT('Ctrl Pts',(-0.264219515132683,20.7629210565933,
-1.42971807191002));
#10432=CARTESIAN_POINT('Ctrl Pts',(0.110909354270868,20.9712543899266,-1.40000000000009));
#10433=CARTESIAN_POINT('Ctrl Pts',(0.486038223674463,21.1795877232599,-1.37028192809016));
#10434=CARTESIAN_POINT('Ctrl Pts',(0.796050318315879,21.3879210565933,-1.15698088816278));
#10435=CARTESIAN_POINT('Ctrl Pts',(1.10606241295736,21.5962543899266,-0.943679848235579));
#10436=CARTESIAN_POINT('Ctrl Pts',(1.26789024243365,21.8045877232599,-0.603949681684177));
#10437=CARTESIAN_POINT('Ctrl Pts',(1.42971807190994,22.0129210565933,-0.264219515132783));
#10438=CARTESIAN_POINT('Ctrl Pts',(1.4,22.2212543899266,0.110909354270855));
#10439=CARTESIAN_POINT('Ctrl Pts',(1.37028192809006,22.42958772326,0.486038223674372));
#10440=CARTESIAN_POINT('Ctrl Pts',(1.15698088816276,22.6379210565933,0.796050318315892));
#10441=CARTESIAN_POINT('Ctrl Pts',(0.943679848235495,22.8462543899266,1.10606241295731));
#10442=CARTESIAN_POINT('Ctrl Pts',(0.603949681684078,23.0545877232599,1.26789024243363));
#10443=CARTESIAN_POINT('Ctrl Pts',(0.264219515132726,23.2629210565933,1.42971807190989));
#10444=CARTESIAN_POINT('Ctrl Pts',(-0.110909354270889,23.4712543899266,
1.39999999999997));
#10445=CARTESIAN_POINT('Ctrl Pts',(-0.48603822367442,23.6795877232599,1.37028192808997));
#10446=CARTESIAN_POINT('Ctrl Pts',(-0.796050318315921,23.8879210565932,
1.15698088816274));
#10447=CARTESIAN_POINT('Ctrl Pts',(-1.10606241295736,24.0962543899266,0.943679848235433));
#10448=CARTESIAN_POINT('Ctrl Pts',(-1.26789024243367,24.3045877232599,0.603949681684089));
#10449=CARTESIAN_POINT('Ctrl Pts',(-1.42971807190992,24.5129210565933,0.264219515132643));
#10450=CARTESIAN_POINT('Ctrl Pts',(-1.40000000000002,24.7212543899266,-0.110909354270923));
#10451=CARTESIAN_POINT('Ctrl Pts',(-1.37028192809004,24.9295877232599,-0.486038223674528));
#10452=CARTESIAN_POINT('Ctrl Pts',(-1.1569808881628,25.1379210565933,-0.796050318315996));
#10453=CARTESIAN_POINT('Ctrl Pts',(-0.943679848235474,25.3462543899266,
-1.10606241295742));
#10454=CARTESIAN_POINT('Ctrl Pts',(-0.60394968168412,25.5545877232599,-1.26789024243365));
#10455=CARTESIAN_POINT('Ctrl Pts',(-0.264219515132702,25.7629210565933,
-1.42971807191003));
#10456=CARTESIAN_POINT('Ctrl Pts',(0.110909354270847,25.9712543899266,-1.40000000000008));
#10457=CARTESIAN_POINT('Ctrl Pts',(0.486038223674463,26.17958772326,-1.37028192809014));
#10458=CARTESIAN_POINT('Ctrl Pts',(0.7960503183159,26.3879210565933,-1.15698088816279));
#10459=CARTESIAN_POINT('Ctrl Pts',(1.10606241295738,26.5962543899266,-0.943679848235541));
#10460=CARTESIAN_POINT('Ctrl Pts',(1.26789024243363,26.80458772326,-0.603949681684177));
#10461=CARTESIAN_POINT('Ctrl Pts',(1.42971807190996,27.0129210565933,-0.264219515132761));
#10462=CARTESIAN_POINT('Ctrl Pts',(1.4,27.2212543899266,0.110909354270855));
#10463=CARTESIAN_POINT('Ctrl Pts',(1.37028192809007,27.42958772326,0.486038223674393));
#10464=CARTESIAN_POINT('Ctrl Pts',(1.15698088816278,27.6379210565933,0.796050318315892));
#10465=CARTESIAN_POINT('Ctrl Pts',(0.943679848235495,27.8462543899266,1.10606241295729));
#10466=CARTESIAN_POINT('Ctrl Pts',(0.603949681684099,28.0545877232599,1.26789024243361));
#10467=CARTESIAN_POINT('Ctrl Pts',(0.264219515132724,28.2629210565933,1.42971807190986));
#10468=CARTESIAN_POINT('Ctrl Pts',(-0.110909354270889,28.4712543899266,
1.39999999999997));
#10469=CARTESIAN_POINT('Ctrl Pts',(-0.48603822367442,28.67958772326,1.37028192808997));
#10470=CARTESIAN_POINT('Ctrl Pts',(-0.796050318315921,28.8879210565933,
1.15698088816275));
#10471=CARTESIAN_POINT('Ctrl Pts',(-1.10606241295734,29.0962543899266,0.943679848235406));
#10472=CARTESIAN_POINT('Ctrl Pts',(-1.26789024243365,29.30458772326,0.603949681684083));
#10473=CARTESIAN_POINT('Ctrl Pts',(-1.42971807190992,29.5129210565933,0.264219515132621));
#10474=CARTESIAN_POINT('Ctrl Pts',(-1.40000000000002,29.7212543899266,-0.110909354270923));
#10475=CARTESIAN_POINT('Ctrl Pts',(-1.37028192809006,29.92958772326,-0.486038223674506));
#10476=CARTESIAN_POINT('Ctrl Pts',(-1.1569808881628,30.1379210565933,-0.796050318315996));
#10477=CARTESIAN_POINT('Ctrl Pts',(-0.943679848235495,30.3462543899266,
-1.10606241295744));
#10478=CARTESIAN_POINT('Ctrl Pts',(-0.60394968168412,30.5545877232599,-1.26789024243366));
#10479=CARTESIAN_POINT('Ctrl Pts',(-0.264219515132702,30.7629210565933,
-1.42971807191004));
#10480=CARTESIAN_POINT('Ctrl Pts',(0.110909354270868,30.9712543899266,-1.40000000000007));
#10481=CARTESIAN_POINT('Ctrl Pts',(0.486038223674439,31.17958772326,-1.37028192809015));
#10482=CARTESIAN_POINT('Ctrl Pts',(0.796050318315879,31.3879210565933,-1.15698088816279));
#10483=CARTESIAN_POINT('Ctrl Pts',(1.10606241295736,31.5962543899266,-0.943679848235557));
#10484=CARTESIAN_POINT('Ctrl Pts',(1.26789024243365,31.80458772326,-0.603949681684177));
#10485=CARTESIAN_POINT('Ctrl Pts',(1.42971807190996,32.0129210565933,-0.264219515132783));
#10486=CARTESIAN_POINT('Ctrl Pts',(1.39999999999998,32.2212543899266,0.11090935427085));
#10487=CARTESIAN_POINT('Ctrl Pts',(1.37028192809008,32.42958772326,0.486038223674377));
#10488=CARTESIAN_POINT('Ctrl Pts',(1.15698088816278,32.6379210565933,0.796050318315892));
#10489=CARTESIAN_POINT('Ctrl Pts',(0.943679848235498,32.8462543899267,1.1060624129573));
#10490=CARTESIAN_POINT('Ctrl Pts',(0.603949681684078,33.05458772326,1.26789024243359));
#10491=CARTESIAN_POINT('Ctrl Pts',(0.264219515132705,33.2629210565933,1.4297180719099));
#10492=CARTESIAN_POINT('Ctrl Pts',(-0.110909354270871,33.4712543899267,
1.39999999999998));
#10493=CARTESIAN_POINT('Ctrl Pts',(-0.486038223674439,33.67958772326,1.37028192808999));
#10494=CARTESIAN_POINT('Ctrl Pts',(-0.796050318315921,33.8879210565933,
1.15698088816275));
#10495=CARTESIAN_POINT('Ctrl Pts',(-1.10606241295736,34.0962543899266,0.943679848235417));
#10496=CARTESIAN_POINT('Ctrl Pts',(-1.26789024243367,34.30458772326,0.603949681684083));
#10497=CARTESIAN_POINT('Ctrl Pts',(-1.42971807190994,34.5129210565933,0.264219515132643));
#10498=CARTESIAN_POINT('Ctrl Pts',(-1.4,34.7212543899266,-0.110909354270923));
#10499=CARTESIAN_POINT('Ctrl Pts',(-1.37028192809004,34.92958772326,-0.486038223674517));
#10500=CARTESIAN_POINT('Ctrl Pts',(-1.1569808881628,35.1379210565933,-0.796050318315944));
#10501=CARTESIAN_POINT('Ctrl Pts',(-0.943679848235495,35.3462543899267,
-1.10606241295742));
#10502=CARTESIAN_POINT('Ctrl Pts',(-0.60394968168412,35.55458772326,-1.26789024243366));
#10503=CARTESIAN_POINT('Ctrl Pts',(-0.26421951513268,35.7629210565933,-1.42971807191003));
#10504=CARTESIAN_POINT('Ctrl Pts',(0.110909354270847,35.9712543899266,-1.40000000000004));
#10505=CARTESIAN_POINT('Ctrl Pts',(0.486038223674442,36.17958772326,-1.37028192809012));
#10506=CARTESIAN_POINT('Ctrl Pts',(0.796050318315903,36.3879210565933,-1.15698088816279));
#10507=CARTESIAN_POINT('Ctrl Pts',(1.10606241295738,36.5962543899266,-0.943679848235568));
#10508=CARTESIAN_POINT('Ctrl Pts',(1.26789024243365,36.80458772326,-0.603949681684162));
#10509=CARTESIAN_POINT('Ctrl Pts',(1.42971807190994,37.0129210565933,-0.264219515132788));
#10510=CARTESIAN_POINT('Ctrl Pts',(1.4,37.2212543899267,0.110909354270845));
#10511=CARTESIAN_POINT('Ctrl Pts',(1.37028192809007,37.42958772326,0.486038223674372));
#10512=CARTESIAN_POINT('Ctrl Pts',(1.15698088816278,37.6379210565933,0.796050318315845));
#10513=CARTESIAN_POINT('Ctrl Pts',(0.943679848235495,37.8462543899266,1.1060624129573));
#10514=CARTESIAN_POINT('Ctrl Pts',(0.603949681684099,38.05458772326,1.26789024243359));
#10515=CARTESIAN_POINT('Ctrl Pts',(0.264219515132702,38.2629210565934,1.42971807190987));
#10516=CARTESIAN_POINT('Ctrl Pts',(-0.110909354270891,38.4712543899267,
1.39999999999999));
#10517=CARTESIAN_POINT('Ctrl Pts',(-0.486038223674442,38.67958772326,1.37028192808997));
#10518=CARTESIAN_POINT('Ctrl Pts',(-0.796050318315942,38.8879210565933,
1.15698088816275));
#10519=CARTESIAN_POINT('Ctrl Pts',(-1.10606241295734,39.0962543899267,0.943679848235401));
#10520=CARTESIAN_POINT('Ctrl Pts',(-1.26789024243367,39.30458772326,0.603949681684089));
#10521=CARTESIAN_POINT('Ctrl Pts',(-1.42971807190992,39.5129210565933,0.264219515132632));
#10522=CARTESIAN_POINT('Ctrl Pts',(-1.40000000000002,39.7212543899266,-0.110909354270923));
#10523=CARTESIAN_POINT('Ctrl Pts',(-2.,-0.27874561007344,-0.110909354270924));
#10524=CARTESIAN_POINT('Ctrl Pts',(-1.97028192809006,-0.0704122767402082,
-0.646807739133109));
#10525=CARTESIAN_POINT('Ctrl Pts',(-1.67659613043344,0.137921056593222,
-1.0960503183159));
#10526=CARTESIAN_POINT('Ctrl Pts',(-1.38291033277682,0.346254389926512,
-1.54529289749873));
#10527=CARTESIAN_POINT('Ctrl Pts',(-0.903949681684104,0.554587723259871,
-1.78750548470438));
#10528=CARTESIAN_POINT('Ctrl Pts',(-0.424989030591367,0.762921056593226,
-2.02971807190993));
#10529=CARTESIAN_POINT('Ctrl Pts',(0.110909354270878,0.971254389926561,
-2.00000000000006));
#10530=CARTESIAN_POINT('Ctrl Pts',(0.646807739133123,1.17958772325984,-1.97028192809007));
#10531=CARTESIAN_POINT('Ctrl Pts',(1.09605031831591,1.38792105659322,-1.67659613043344));
#10532=CARTESIAN_POINT('Ctrl Pts',(1.54529289749868,1.59625438992652,-1.38291033277687));
#10533=CARTESIAN_POINT('Ctrl Pts',(1.78750548470428,1.80458772325989,-0.903949681684113));
#10534=CARTESIAN_POINT('Ctrl Pts',(2.02971807190996,2.01292105659317,-0.42498903059139));
#10535=CARTESIAN_POINT('Ctrl Pts',(2.,2.22125438992656,0.110909354270855));
#10536=CARTESIAN_POINT('Ctrl Pts',(1.97028192809007,2.42958772325984,0.646807739133102));
#10537=CARTESIAN_POINT('Ctrl Pts',(1.67659613043345,2.63792105659317,1.09605031831587));
#10538=CARTESIAN_POINT('Ctrl Pts',(1.38291033277682,2.8462543899265,1.54529289749866));
#10539=CARTESIAN_POINT('Ctrl Pts',(0.903949681684104,3.0545877232599,1.78750548470426));
#10540=CARTESIAN_POINT('Ctrl Pts',(0.424989030591383,3.26292105659317,2.02971807190993));
#10541=CARTESIAN_POINT('Ctrl Pts',(-0.11090935427085,3.47125438992654,1.99999999999995));
#10542=CARTESIAN_POINT('Ctrl Pts',(-0.646807739133109,3.67958772325983,
1.97028192809007));
#10543=CARTESIAN_POINT('Ctrl Pts',(-1.0960503183159,3.88792105659323,1.67659613043343));
#10544=CARTESIAN_POINT('Ctrl Pts',(-1.54529289749868,4.09625438992648,1.38291033277681));
#10545=CARTESIAN_POINT('Ctrl Pts',(-1.78750548470431,4.30458772325989,0.903949681684051));
#10546=CARTESIAN_POINT('Ctrl Pts',(-2.02971807190994,4.51292105659318,0.424989030591333));
#10547=CARTESIAN_POINT('Ctrl Pts',(-2.,4.72125438992654,-0.110909354270966));
#10548=CARTESIAN_POINT('Ctrl Pts',(-1.97028192809006,4.92958772325984,-0.646807739133087));
#10549=CARTESIAN_POINT('Ctrl Pts',(-1.67659613043343,5.13792105659321,-1.09605031831595));
#10550=CARTESIAN_POINT('Ctrl Pts',(-1.38291033277682,5.34625438992653,-1.54529289749872));
#10551=CARTESIAN_POINT('Ctrl Pts',(-0.903949681684091,5.5545877232599,-1.78750548470436));
#10552=CARTESIAN_POINT('Ctrl Pts',(-0.424989030591382,5.76292105659322,
-2.02971807190993));
#10553=CARTESIAN_POINT('Ctrl Pts',(0.110909354270865,5.97125438992659,-2.00000000000009));
#10554=CARTESIAN_POINT('Ctrl Pts',(0.64680773913311,6.17958772325983,-1.97028192809005));
#10555=CARTESIAN_POINT('Ctrl Pts',(1.0960503183159,6.38792105659326,-1.67659613043349));
#10556=CARTESIAN_POINT('Ctrl Pts',(1.54529289749868,6.5962543899265,-1.38291033277683));
#10557=CARTESIAN_POINT('Ctrl Pts',(1.7875054847043,6.80458772325989,-0.903949681684162));
#10558=CARTESIAN_POINT('Ctrl Pts',(2.02971807190991,7.01292105659322,-0.424989030591398));
#10559=CARTESIAN_POINT('Ctrl Pts',(2.,7.22125438992656,0.110909354270862));
#10560=CARTESIAN_POINT('Ctrl Pts',(1.97028192809006,7.42958772325989,0.646807739133109));
#10561=CARTESIAN_POINT('Ctrl Pts',(1.67659613043344,7.63792105659322,1.09605031831585));
#10562=CARTESIAN_POINT('Ctrl Pts',(1.38291033277683,7.84625438992656,1.54529289749869));
#10563=CARTESIAN_POINT('Ctrl Pts',(0.903949681684104,8.05458772325989,1.78750548470431));
#10564=CARTESIAN_POINT('Ctrl Pts',(0.424989030591398,8.26292105659318,2.02971807190991));
#10565=CARTESIAN_POINT('Ctrl Pts',(-0.110909354270878,8.47125438992655,
1.99999999999995));
#10566=CARTESIAN_POINT('Ctrl Pts',(-0.646807739133123,8.67958772325983,
1.97028192809004));
#10567=CARTESIAN_POINT('Ctrl Pts',(-1.0960503183159,8.88792105659324,1.67659613043339));
#10568=CARTESIAN_POINT('Ctrl Pts',(-1.54529289749868,9.0962543899265,1.38291033277682));
#10569=CARTESIAN_POINT('Ctrl Pts',(-1.78750548470431,9.3045877232599,0.903949681684085));
#10570=CARTESIAN_POINT('Ctrl Pts',(-2.02971807190993,9.51292105659317,0.424989030591355));
#10571=CARTESIAN_POINT('Ctrl Pts',(-2.,9.72125438992657,-0.110909354270924));
#10572=CARTESIAN_POINT('Ctrl Pts',(-1.97028192809007,9.92958772325983,-0.646807739133123));
#10573=CARTESIAN_POINT('Ctrl Pts',(-1.67659613043344,10.1379210565932,-1.09605031831599));
#10574=CARTESIAN_POINT('Ctrl Pts',(-1.38291033277681,10.3462543899265,-1.54529289749875));
#10575=CARTESIAN_POINT('Ctrl Pts',(-0.903949681684116,10.5545877232599,
-1.78750548470438));
#10576=CARTESIAN_POINT('Ctrl Pts',(-0.424989030591382,10.7629210565932,
-2.02971807190998));
#10577=CARTESIAN_POINT('Ctrl Pts',(0.110909354270878,10.9712543899266,-2.00000000000009));
#10578=CARTESIAN_POINT('Ctrl Pts',(0.646807739133123,11.1795877232599,-1.97028192809007));
#10579=CARTESIAN_POINT('Ctrl Pts',(1.09605031831591,11.3879210565932,-1.67659613043351));
#10580=CARTESIAN_POINT('Ctrl Pts',(1.54529289749868,11.5962543899265,-1.38291033277682));
#10581=CARTESIAN_POINT('Ctrl Pts',(1.78750548470431,11.8045877232599,-0.903949681684182));
#10582=CARTESIAN_POINT('Ctrl Pts',(2.02971807190993,12.0129210565932,-0.424989030591383));
#10583=CARTESIAN_POINT('Ctrl Pts',(2.,12.2212543899266,0.110909354270862));
#10584=CARTESIAN_POINT('Ctrl Pts',(1.97028192809007,12.4295877232599,0.646807739133051));
#10585=CARTESIAN_POINT('Ctrl Pts',(1.67659613043345,12.6379210565932,1.09605031831589));
#10586=CARTESIAN_POINT('Ctrl Pts',(1.38291033277683,12.8462543899266,1.54529289749867));
#10587=CARTESIAN_POINT('Ctrl Pts',(0.903949681684118,13.0545877232599,1.78750548470425));
#10588=CARTESIAN_POINT('Ctrl Pts',(0.424989030591382,13.2629210565932,2.02971807190993));
#10589=CARTESIAN_POINT('Ctrl Pts',(-0.110909354270864,13.4712543899266,
1.99999999999997));
#10590=CARTESIAN_POINT('Ctrl Pts',(-0.646807739133109,13.6795877232599,
1.97028192809006));
#10591=CARTESIAN_POINT('Ctrl Pts',(-1.0960503183159,13.8879210565932,1.67659613043339));
#10592=CARTESIAN_POINT('Ctrl Pts',(-1.54529289749868,14.0962543899266,1.38291033277682));
#10593=CARTESIAN_POINT('Ctrl Pts',(-1.7875054847043,14.3045877232599,0.903949681684092));
#10594=CARTESIAN_POINT('Ctrl Pts',(-2.02971807190993,14.5129210565932,0.424989030591326));
#10595=CARTESIAN_POINT('Ctrl Pts',(-2.,14.7212543899266,-0.110909354270938));
#10596=CARTESIAN_POINT('Ctrl Pts',(-1.97028192809006,14.9295877232599,-0.646807739133109));
#10597=CARTESIAN_POINT('Ctrl Pts',(-1.67659613043344,15.1379210565933,-1.09605031831595));
#10598=CARTESIAN_POINT('Ctrl Pts',(-1.38291033277683,15.3462543899265,-1.54529289749874));
#10599=CARTESIAN_POINT('Ctrl Pts',(-0.903949681684104,15.5545877232599,
-1.78750548470439));
#10600=CARTESIAN_POINT('Ctrl Pts',(-0.424989030591382,15.7629210565932,
-2.02971807190993));
#10601=CARTESIAN_POINT('Ctrl Pts',(0.110909354270852,15.9712543899266,-2.00000000000006));
#10602=CARTESIAN_POINT('Ctrl Pts',(0.646807739133109,16.1795877232599,-1.97028192809006));
#10603=CARTESIAN_POINT('Ctrl Pts',(1.0960503183159,16.3879210565933,-1.67659613043349));
#10604=CARTESIAN_POINT('Ctrl Pts',(1.5452928974987,16.5962543899265,-1.38291033277688));
#10605=CARTESIAN_POINT('Ctrl Pts',(1.78750548470431,16.8045877232599,-0.903949681684148));
#10606=CARTESIAN_POINT('Ctrl Pts',(2.02971807190993,17.0129210565932,-0.424989030591383));
#10607=CARTESIAN_POINT('Ctrl Pts',(2.,17.2212543899266,0.110909354270813));
#10608=CARTESIAN_POINT('Ctrl Pts',(1.97028192809007,17.4295877232599,0.646807739133109));
#10609=CARTESIAN_POINT('Ctrl Pts',(1.67659613043345,17.6379210565933,1.09605031831585));
#10610=CARTESIAN_POINT('Ctrl Pts',(1.38291033277684,17.8462543899265,1.54529289749865));
#10611=CARTESIAN_POINT('Ctrl Pts',(0.903949681684104,18.0545877232599,1.78750548470431));
#10612=CARTESIAN_POINT('Ctrl Pts',(0.424989030591369,18.2629210565932,2.02971807190994));
#10613=CARTESIAN_POINT('Ctrl Pts',(-0.110909354270865,18.4712543899266,
2.));
#10614=CARTESIAN_POINT('Ctrl Pts',(-0.646807739133109,18.6795877232599,
1.97028192809006));
#10615=CARTESIAN_POINT('Ctrl Pts',(-1.0960503183159,18.8879210565933,1.6765961304334));
#10616=CARTESIAN_POINT('Ctrl Pts',(-1.54529289749867,19.0962543899266,1.38291033277682));
#10617=CARTESIAN_POINT('Ctrl Pts',(-1.78750548470431,19.3045877232599,0.903949681684071));
#10618=CARTESIAN_POINT('Ctrl Pts',(-2.02971807190993,19.5129210565932,0.42498903059134));
#10619=CARTESIAN_POINT('Ctrl Pts',(-2.,19.7212543899266,-0.110909354270924));
#10620=CARTESIAN_POINT('Ctrl Pts',(-1.97028192809006,19.9295877232599,-0.646807739133152));
#10621=CARTESIAN_POINT('Ctrl Pts',(-1.67659613043345,20.1379210565933,-1.09605031831597));
#10622=CARTESIAN_POINT('Ctrl Pts',(-1.38291033277682,20.3462543899266,-1.54529289749875));
#10623=CARTESIAN_POINT('Ctrl Pts',(-0.903949681684103,20.5545877232599,
-1.78750548470438));
#10624=CARTESIAN_POINT('Ctrl Pts',(-0.424989030591367,20.7629210565932,
-2.02971807190997));
#10625=CARTESIAN_POINT('Ctrl Pts',(0.110909354270864,20.9712543899266,-2.0000000000001));
#10626=CARTESIAN_POINT('Ctrl Pts',(0.64680773913311,21.1795877232599,-1.97028192809011));
#10627=CARTESIAN_POINT('Ctrl Pts',(1.0960503183159,21.3879210565933,-1.67659613043352));
#10628=CARTESIAN_POINT('Ctrl Pts',(1.54529289749868,21.5962543899266,-1.38291033277682));
#10629=CARTESIAN_POINT('Ctrl Pts',(1.78750548470431,21.8045877232599,-0.90394968168419));
#10630=CARTESIAN_POINT('Ctrl Pts',(2.02971807190991,22.0129210565932,-0.42498903059139));
#10631=CARTESIAN_POINT('Ctrl Pts',(2.,22.2212543899266,0.110909354270855));
#10632=CARTESIAN_POINT('Ctrl Pts',(1.9702819280901,22.4295877232599,0.646807739133087));
#10633=CARTESIAN_POINT('Ctrl Pts',(1.67659613043345,22.6379210565933,1.09605031831588));
#10634=CARTESIAN_POINT('Ctrl Pts',(1.38291033277683,22.8462543899266,1.54529289749862));
#10635=CARTESIAN_POINT('Ctrl Pts',(0.903949681684118,23.0545877232599,1.78750548470426));
#10636=CARTESIAN_POINT('Ctrl Pts',(0.424989030591383,23.2629210565932,2.02971807190993));
#10637=CARTESIAN_POINT('Ctrl Pts',(-0.110909354270864,23.4712543899266,
1.99999999999997));
#10638=CARTESIAN_POINT('Ctrl Pts',(-0.646807739133109,23.6795877232599,
1.97028192809003));
#10639=CARTESIAN_POINT('Ctrl Pts',(-1.09605031831588,23.8879210565933,1.67659613043339));
#10640=CARTESIAN_POINT('Ctrl Pts',(-1.54529289749869,24.0962543899266,1.38291033277682));
#10641=CARTESIAN_POINT('Ctrl Pts',(-1.78750548470431,24.3045877232599,0.903949681684092));
#10642=CARTESIAN_POINT('Ctrl Pts',(-2.02971807190995,24.5129210565932,0.424989030591319));
#10643=CARTESIAN_POINT('Ctrl Pts',(-2.,24.7212543899266,-0.110909354270938));
#10644=CARTESIAN_POINT('Ctrl Pts',(-1.97028192809005,24.9295877232599,-0.646807739133109));
#10645=CARTESIAN_POINT('Ctrl Pts',(-1.67659613043344,25.1379210565933,-1.09605031831594));
#10646=CARTESIAN_POINT('Ctrl Pts',(-1.38291033277682,25.3462543899266,-1.54529289749872));
#10647=CARTESIAN_POINT('Ctrl Pts',(-0.903949681684104,25.55458772326,-1.7875054847044));
#10648=CARTESIAN_POINT('Ctrl Pts',(-0.424989030591382,25.7629210565933,
-2.02971807190993));
#10649=CARTESIAN_POINT('Ctrl Pts',(0.110909354270864,25.9712543899266,-2.00000000000006));
#10650=CARTESIAN_POINT('Ctrl Pts',(0.646807739133109,26.1795877232599,-1.97028192809006));
#10651=CARTESIAN_POINT('Ctrl Pts',(1.0960503183159,26.3879210565933,-1.67659613043348));
#10652=CARTESIAN_POINT('Ctrl Pts',(1.5452928974987,26.5962543899266,-1.38291033277687));
#10653=CARTESIAN_POINT('Ctrl Pts',(1.78750548470431,26.80458772326,-0.903949681684155));
#10654=CARTESIAN_POINT('Ctrl Pts',(2.02971807190993,27.0129210565933,-0.424989030591383));
#10655=CARTESIAN_POINT('Ctrl Pts',(2.00000000000003,27.2212543899266,0.11090935427082));
#10656=CARTESIAN_POINT('Ctrl Pts',(1.97028192809007,27.4295877232599,0.646807739133109));
#10657=CARTESIAN_POINT('Ctrl Pts',(1.67659613043345,27.6379210565933,1.09605031831587));
#10658=CARTESIAN_POINT('Ctrl Pts',(1.38291033277684,27.8462543899266,1.54529289749868));
#10659=CARTESIAN_POINT('Ctrl Pts',(0.903949681684103,28.0545877232599,1.78750548470431));
#10660=CARTESIAN_POINT('Ctrl Pts',(0.424989030591382,28.2629210565932,2.02971807190993));
#10661=CARTESIAN_POINT('Ctrl Pts',(-0.110909354270852,28.4712543899266,
1.99999999999998));
#10662=CARTESIAN_POINT('Ctrl Pts',(-0.646807739133109,28.6795877232599,
1.97028192809006));
#10663=CARTESIAN_POINT('Ctrl Pts',(-1.0960503183159,28.8879210565933,1.67659613043341));
#10664=CARTESIAN_POINT('Ctrl Pts',(-1.54529289749868,29.0962543899266,1.38291033277682));
#10665=CARTESIAN_POINT('Ctrl Pts',(-1.78750548470432,29.30458772326,0.903949681684071));
#10666=CARTESIAN_POINT('Ctrl Pts',(-2.02971807190993,29.5129210565933,0.42498903059134));
#10667=CARTESIAN_POINT('Ctrl Pts',(-2.,29.7212543899266,-0.110909354270917));
#10668=CARTESIAN_POINT('Ctrl Pts',(-1.97028192809006,29.9295877232599,-0.646807739133087));
#10669=CARTESIAN_POINT('Ctrl Pts',(-1.67659613043345,30.1379210565933,-1.09605031831597));
#10670=CARTESIAN_POINT('Ctrl Pts',(-1.38291033277683,30.3462543899266,-1.54529289749872));
#10671=CARTESIAN_POINT('Ctrl Pts',(-0.903949681684103,30.55458772326,-1.78750548470437));
#10672=CARTESIAN_POINT('Ctrl Pts',(-0.424989030591367,30.7629210565933,
-2.02971807190996));
#10673=CARTESIAN_POINT('Ctrl Pts',(0.110909354270865,30.9712543899266,-2.00000000000009));
#10674=CARTESIAN_POINT('Ctrl Pts',(0.646807739133123,31.1795877232599,-1.97028192809004));
#10675=CARTESIAN_POINT('Ctrl Pts',(1.0960503183159,31.3879210565933,-1.67659613043352));
#10676=CARTESIAN_POINT('Ctrl Pts',(1.54529289749868,31.5962543899266,-1.38291033277685));
#10677=CARTESIAN_POINT('Ctrl Pts',(1.78750548470431,31.80458772326,-0.903949681684169));
#10678=CARTESIAN_POINT('Ctrl Pts',(2.02971807190993,32.0129210565933,-0.424989030591419));
#10679=CARTESIAN_POINT('Ctrl Pts',(2.,32.2212543899266,0.110909354270869));
#10680=CARTESIAN_POINT('Ctrl Pts',(1.97028192809004,32.4295877232599,0.646807739133087));
#10681=CARTESIAN_POINT('Ctrl Pts',(1.67659613043345,32.6379210565933,1.09605031831587));
#10682=CARTESIAN_POINT('Ctrl Pts',(1.38291033277682,32.8462543899266,1.54529289749868));
#10683=CARTESIAN_POINT('Ctrl Pts',(0.903949681684104,33.0545877232599,1.78750548470431));
#10684=CARTESIAN_POINT('Ctrl Pts',(0.424989030591383,33.2629210565932,2.02971807190993));
#10685=CARTESIAN_POINT('Ctrl Pts',(-0.110909354270864,33.4712543899267,
1.99999999999997));
#10686=CARTESIAN_POINT('Ctrl Pts',(-0.646807739133109,33.6795877232599,
1.97028192809004));
#10687=CARTESIAN_POINT('Ctrl Pts',(-1.09605031831588,33.8879210565934,1.6765961304334));
#10688=CARTESIAN_POINT('Ctrl Pts',(-1.54529289749868,34.0962543899266,1.38291033277683));
#10689=CARTESIAN_POINT('Ctrl Pts',(-1.78750548470431,34.30458772326,0.903949681684037));
#10690=CARTESIAN_POINT('Ctrl Pts',(-2.02971807190994,34.5129210565932,0.424989030591383));
#10691=CARTESIAN_POINT('Ctrl Pts',(-2.,34.7212543899267,-0.110909354270938));
#10692=CARTESIAN_POINT('Ctrl Pts',(-1.97028192809006,34.9295877232599,-0.646807739133123));
#10693=CARTESIAN_POINT('Ctrl Pts',(-1.67659613043344,35.1379210565933,-1.09605031831594));
#10694=CARTESIAN_POINT('Ctrl Pts',(-1.38291033277682,35.3462543899267,-1.54529289749875));
#10695=CARTESIAN_POINT('Ctrl Pts',(-0.903949681684103,35.55458772326,-1.78750548470439));
#10696=CARTESIAN_POINT('Ctrl Pts',(-0.424989030591382,35.7629210565932,
-2.02971807190993));
#10697=CARTESIAN_POINT('Ctrl Pts',(0.110909354270864,35.9712543899267,-2.00000000000003));
#10698=CARTESIAN_POINT('Ctrl Pts',(0.64680773913311,36.1795877232599,-1.97028192809006));
#10699=CARTESIAN_POINT('Ctrl Pts',(1.0960503183159,36.3879210565933,-1.67659613043348));
#10700=CARTESIAN_POINT('Ctrl Pts',(1.54529289749869,36.5962543899266,-1.38291033277682));
#10701=CARTESIAN_POINT('Ctrl Pts',(1.78750548470431,36.80458772326,-0.903949681684127));
#10702=CARTESIAN_POINT('Ctrl Pts',(2.02971807190993,37.0129210565932,-0.424989030591383));
#10703=CARTESIAN_POINT('Ctrl Pts',(2.,37.2212543899267,0.110909354270834));
#10704=CARTESIAN_POINT('Ctrl Pts',(1.97028192809006,37.4295877232599,0.646807739133109));
#10705=CARTESIAN_POINT('Ctrl Pts',(1.67659613043345,37.6379210565933,1.09605031831588));
#10706=CARTESIAN_POINT('Ctrl Pts',(1.38291033277681,37.8462543899266,1.54529289749865));
#10707=CARTESIAN_POINT('Ctrl Pts',(0.903949681684104,38.0545877232599,1.78750548470431));
#10708=CARTESIAN_POINT('Ctrl Pts',(0.424989030591383,38.2629210565933,2.02971807190991));
#10709=CARTESIAN_POINT('Ctrl Pts',(-0.11090935427085,38.4712543899266,1.99999999999995));
#10710=CARTESIAN_POINT('Ctrl Pts',(-0.64680773913311,38.67958772326,1.97028192809006));
#10711=CARTESIAN_POINT('Ctrl Pts',(-1.0960503183159,38.8879210565933,1.67659613043344));
#10712=CARTESIAN_POINT('Ctrl Pts',(-1.54529289749868,39.0962543899266,1.38291033277682));
#10713=CARTESIAN_POINT('Ctrl Pts',(-1.78750548470431,39.30458772326,0.903949681684064));
#10714=CARTESIAN_POINT('Ctrl Pts',(-2.02971807190993,39.5129210565932,0.424989030591369));
#10715=CARTESIAN_POINT('Ctrl Pts',(-2.,39.7212543899267,-0.110909354270917));
#10716=CARTESIAN_POINT('Ctrl Pts',(-2.6,-0.278745610073447,-0.11090935427086));
#10717=CARTESIAN_POINT('Ctrl Pts',(-2.57028192809005,-0.0704122767401095,
-0.807577254591869));
#10718=CARTESIAN_POINT('Ctrl Pts',(-2.19621137270411,0.137921056593207,
-1.39605031831597));
#10719=CARTESIAN_POINT('Ctrl Pts',(-1.82214081731814,0.346254389926554,
-1.98452338204009));
#10720=CARTESIAN_POINT('Ctrl Pts',(-1.20394968168411,0.554587723259855,
-2.30712072697501));
#10721=CARTESIAN_POINT('Ctrl Pts',(-0.585758546050059,0.762921056593228,
-2.62971807191003));
#10722=CARTESIAN_POINT('Ctrl Pts',(0.11090935427086,0.971254389926535,-2.60000000000008));
#10723=CARTESIAN_POINT('Ctrl Pts',(0.807577254591799,1.17958772325987,-2.57028192809015));
#10724=CARTESIAN_POINT('Ctrl Pts',(1.39605031831589,1.38792105659322,-2.19621137270419));
#10725=CARTESIAN_POINT('Ctrl Pts',(1.98452338204001,1.59625438992655,-1.82214081731816));
#10726=CARTESIAN_POINT('Ctrl Pts',(2.30712072697495,1.80458772325989,-1.20394968168416));
#10727=CARTESIAN_POINT('Ctrl Pts',(2.62971807190993,2.01292105659322,-0.585758546050151));
#10728=CARTESIAN_POINT('Ctrl Pts',(2.59999999999998,2.22125438992652,0.110909354270808));
#10729=CARTESIAN_POINT('Ctrl Pts',(2.57028192809007,2.42958772325989,0.807577254591686));
#10730=CARTESIAN_POINT('Ctrl Pts',(2.19621137270409,2.63792105659321,1.39605031831586));
#10731=CARTESIAN_POINT('Ctrl Pts',(1.82214081731816,2.84625438992655,1.98452338203998));
#10732=CARTESIAN_POINT('Ctrl Pts',(1.20394968168409,3.05458772325989,2.30712072697489));
#10733=CARTESIAN_POINT('Ctrl Pts',(0.585758546050062,3.26292105659321,2.62971807190987));
#10734=CARTESIAN_POINT('Ctrl Pts',(-0.11090935427086,3.47125438992654,2.59999999999991));
#10735=CARTESIAN_POINT('Ctrl Pts',(-0.807577254591778,3.67958772325991,
2.57028192809));
#10736=CARTESIAN_POINT('Ctrl Pts',(-1.39605031831589,3.8879210565932,2.19621137270409));
#10737=CARTESIAN_POINT('Ctrl Pts',(-1.98452338203998,4.09625438992658,1.82214081731811));
#10738=CARTESIAN_POINT('Ctrl Pts',(-2.30712072697499,4.30458772325988,1.20394968168402));
#10739=CARTESIAN_POINT('Ctrl Pts',(-2.62971807190992,4.51292105659321,0.585758546049978));
#10740=CARTESIAN_POINT('Ctrl Pts',(-2.6,4.72125438992652,-0.110909354270855));
#10741=CARTESIAN_POINT('Ctrl Pts',(-2.57028192809005,4.92958772325988,-0.807577254591864));
#10742=CARTESIAN_POINT('Ctrl Pts',(-2.19621137270413,5.13792105659322,-1.39605031831589));
#10743=CARTESIAN_POINT('Ctrl Pts',(-1.82214081731815,5.34625438992655,-1.98452338204009));
#10744=CARTESIAN_POINT('Ctrl Pts',(-1.20394968168413,5.55458772325989,-2.30712072697498));
#10745=CARTESIAN_POINT('Ctrl Pts',(-0.585758546050059,5.76292105659322,
-2.62971807191006));
#10746=CARTESIAN_POINT('Ctrl Pts',(0.110909354270839,5.97125438992656,-2.6));
#10747=CARTESIAN_POINT('Ctrl Pts',(0.807577254591799,6.1795877232599,-2.57028192809015));
#10748=CARTESIAN_POINT('Ctrl Pts',(1.39605031831589,6.38792105659324,-2.19621137270419));
#10749=CARTESIAN_POINT('Ctrl Pts',(1.98452338204003,6.59625438992657,-1.82214081731824));
#10750=CARTESIAN_POINT('Ctrl Pts',(2.30712072697497,6.80458772325989,-1.20394968168419));
#10751=CARTESIAN_POINT('Ctrl Pts',(2.62971807190993,7.01292105659322,-0.58575854605014));
#10752=CARTESIAN_POINT('Ctrl Pts',(2.6,7.22125438992658,0.110909354270855));
#10753=CARTESIAN_POINT('Ctrl Pts',(2.57028192809009,7.42958772325989,0.807577254591767));
#10754=CARTESIAN_POINT('Ctrl Pts',(2.19621137270411,7.63792105659324,1.39605031831581));
#10755=CARTESIAN_POINT('Ctrl Pts',(1.82214081731816,7.84625438992655,1.98452338203995));
#10756=CARTESIAN_POINT('Ctrl Pts',(1.20394968168409,8.05458772325989,2.30712072697495));
#10757=CARTESIAN_POINT('Ctrl Pts',(0.585758546050062,8.26292105659324,2.62971807190983));
#10758=CARTESIAN_POINT('Ctrl Pts',(-0.11090935427086,8.47125438992656,2.59999999999999));
#10759=CARTESIAN_POINT('Ctrl Pts',(-0.807577254591772,8.67958772325989,
2.57028192809002));
#10760=CARTESIAN_POINT('Ctrl Pts',(-1.39605031831589,8.88792105659322,2.1962113727041));
#10761=CARTESIAN_POINT('Ctrl Pts',(-1.98452338203998,9.09625438992657,1.82214081731807));
#10762=CARTESIAN_POINT('Ctrl Pts',(-2.30712072697499,9.30458772325988,1.20394968168402));
#10763=CARTESIAN_POINT('Ctrl Pts',(-2.62971807190992,9.51292105659323,0.585758546050059));
#10764=CARTESIAN_POINT('Ctrl Pts',(-2.6,9.72125438992655,-0.11090935427086));
#10765=CARTESIAN_POINT('Ctrl Pts',(-2.57028192809007,9.92958772325989,-0.80757725459195));
#10766=CARTESIAN_POINT('Ctrl Pts',(-2.19621137270412,10.1379210565932,-1.39605031831597));
#10767=CARTESIAN_POINT('Ctrl Pts',(-1.82214081731816,10.3462543899266,-1.98452338204001));
#10768=CARTESIAN_POINT('Ctrl Pts',(-1.20394968168413,10.5545877232599,-2.30712072697498));
#10769=CARTESIAN_POINT('Ctrl Pts',(-0.585758546050059,10.7629210565933,
-2.62971807191005));
#10770=CARTESIAN_POINT('Ctrl Pts',(0.11090935427086,10.9712543899266,-2.6));
#10771=CARTESIAN_POINT('Ctrl Pts',(0.80757725459178,11.1795877232599,-2.57028192809015));
#10772=CARTESIAN_POINT('Ctrl Pts',(1.39605031831587,11.3879210565932,-2.19621137270419));
#10773=CARTESIAN_POINT('Ctrl Pts',(1.98452338204001,11.5962543899266,-1.82214081731816));
#10774=CARTESIAN_POINT('Ctrl Pts',(2.30712072697495,11.8045877232599,-1.20394968168419));
#10775=CARTESIAN_POINT('Ctrl Pts',(2.62971807190993,12.0129210565933,-0.585758546050162));
#10776=CARTESIAN_POINT('Ctrl Pts',(2.6,12.2212543899266,0.11090935427085));
#10777=CARTESIAN_POINT('Ctrl Pts',(2.57028192809007,12.4295877232599,0.807577254591702));
#10778=CARTESIAN_POINT('Ctrl Pts',(2.19621137270409,12.6379210565932,1.39605031831582));
#10779=CARTESIAN_POINT('Ctrl Pts',(1.82214081731816,12.8462543899266,1.98452338203998));
#10780=CARTESIAN_POINT('Ctrl Pts',(1.20394968168411,13.0545877232599,2.30712072697493));
#10781=CARTESIAN_POINT('Ctrl Pts',(0.585758546050084,13.2629210565932,2.62971807190985));
#10782=CARTESIAN_POINT('Ctrl Pts',(-0.11090935427086,13.4712543899266,2.59999999999995));
#10783=CARTESIAN_POINT('Ctrl Pts',(-0.807577254591778,13.6795877232599,
2.57028192809));
#10784=CARTESIAN_POINT('Ctrl Pts',(-1.39605031831591,13.8879210565933,2.19621137270409));
#10785=CARTESIAN_POINT('Ctrl Pts',(-1.98452338204001,14.0962543899266,1.82214081731811));
#10786=CARTESIAN_POINT('Ctrl Pts',(-2.30712072697499,14.3045877232599,1.20394968168402));
#10787=CARTESIAN_POINT('Ctrl Pts',(-2.62971807190992,14.5129210565932,0.585758546049984));
#10788=CARTESIAN_POINT('Ctrl Pts',(-2.60000000000002,14.7212543899266,-0.110909354270865));
#10789=CARTESIAN_POINT('Ctrl Pts',(-2.57028192809007,14.9295877232599,-0.807577254591869));
#10790=CARTESIAN_POINT('Ctrl Pts',(-2.19621137270411,15.1379210565932,-1.39605031831597));
#10791=CARTESIAN_POINT('Ctrl Pts',(-1.82214081731815,15.3462543899266,-1.98452338204009));
#10792=CARTESIAN_POINT('Ctrl Pts',(-1.20394968168413,15.5545877232599,-2.30712072697498));
#10793=CARTESIAN_POINT('Ctrl Pts',(-0.58575854605004,15.7629210565933,-2.62971807191003));
#10794=CARTESIAN_POINT('Ctrl Pts',(0.110909354270839,15.9712543899266,-2.6));
#10795=CARTESIAN_POINT('Ctrl Pts',(0.807577254591799,16.1795877232599,-2.57028192809018));
#10796=CARTESIAN_POINT('Ctrl Pts',(1.39605031831589,16.3879210565933,-2.19621137270417));
#10797=CARTESIAN_POINT('Ctrl Pts',(1.98452338204002,16.5962543899266,-1.82214081731817));
#10798=CARTESIAN_POINT('Ctrl Pts',(2.30712072697497,16.8045877232599,-1.20394968168419));
#10799=CARTESIAN_POINT('Ctrl Pts',(2.62971807190995,17.0129210565933,-0.585758546050151));
#10800=CARTESIAN_POINT('Ctrl Pts',(2.59999999999998,17.2212543899266,0.110909354270855));
#10801=CARTESIAN_POINT('Ctrl Pts',(2.57028192809007,17.42958772326,0.807577254591713));
#10802=CARTESIAN_POINT('Ctrl Pts',(2.19621137270409,17.6379210565933,1.39605031831588));
#10803=CARTESIAN_POINT('Ctrl Pts',(1.82214081731816,17.8462543899266,1.98452338203995));
#10804=CARTESIAN_POINT('Ctrl Pts',(1.20394968168411,18.0545877232599,2.30712072697492));
#10805=CARTESIAN_POINT('Ctrl Pts',(0.585758546050062,18.2629210565933,2.62971807190985));
#10806=CARTESIAN_POINT('Ctrl Pts',(-0.11090935427086,18.4712543899266,2.59999999999995));
#10807=CARTESIAN_POINT('Ctrl Pts',(-0.807577254591775,18.6795877232599,
2.57028192809003));
#10808=CARTESIAN_POINT('Ctrl Pts',(-1.39605031831589,18.8879210565933,2.19621137270408));
#10809=CARTESIAN_POINT('Ctrl Pts',(-1.98452338204001,19.0962543899266,1.82214081731808));
#10810=CARTESIAN_POINT('Ctrl Pts',(-2.30712072697499,19.3045877232599,1.2039496816841));
#10811=CARTESIAN_POINT('Ctrl Pts',(-2.62971807190991,19.5129210565933,0.585758546050022));
#10812=CARTESIAN_POINT('Ctrl Pts',(-2.6,19.7212543899266,-0.110909354270865));
#10813=CARTESIAN_POINT('Ctrl Pts',(-2.57028192809005,19.9295877232599,-0.807577254591831));
#10814=CARTESIAN_POINT('Ctrl Pts',(-2.19621137270411,20.1379210565933,-1.39605031831597));
#10815=CARTESIAN_POINT('Ctrl Pts',(-1.82214081731814,20.3462543899266,-1.98452338204008));
#10816=CARTESIAN_POINT('Ctrl Pts',(-1.20394968168413,20.5545877232599,-2.30712072697501));
#10817=CARTESIAN_POINT('Ctrl Pts',(-0.585758546050059,20.7629210565933,
-2.62971807191003));
#10818=CARTESIAN_POINT('Ctrl Pts',(0.110909354270839,20.9712543899266,-2.6));
#10819=CARTESIAN_POINT('Ctrl Pts',(0.80757725459178,21.1795877232599,-2.57028192809016));
#10820=CARTESIAN_POINT('Ctrl Pts',(1.39605031831587,21.3879210565933,-2.19621137270417));
#10821=CARTESIAN_POINT('Ctrl Pts',(1.98452338204003,21.5962543899266,-1.82214081731822));
#10822=CARTESIAN_POINT('Ctrl Pts',(2.30712072697495,21.8045877232599,-1.20394968168419));
#10823=CARTESIAN_POINT('Ctrl Pts',(2.62971807190993,22.0129210565933,-0.585758546050135));
#10824=CARTESIAN_POINT('Ctrl Pts',(2.6,22.2212543899266,0.11090935427085));
#10825=CARTESIAN_POINT('Ctrl Pts',(2.57028192809009,22.42958772326,0.807577254591702));
#10826=CARTESIAN_POINT('Ctrl Pts',(2.19621137270411,22.6379210565933,1.39605031831588));
#10827=CARTESIAN_POINT('Ctrl Pts',(1.82214081731818,22.8462543899266,1.98452338203997));
#10828=CARTESIAN_POINT('Ctrl Pts',(1.20394968168411,23.0545877232599,2.30712072697493));
#10829=CARTESIAN_POINT('Ctrl Pts',(0.585758546050081,23.2629210565933,2.62971807190987));
#10830=CARTESIAN_POINT('Ctrl Pts',(-0.110909354270881,23.4712543899266,
2.59999999999995));
#10831=CARTESIAN_POINT('Ctrl Pts',(-0.807577254591756,23.6795877232599,
2.57028192809001));
#10832=CARTESIAN_POINT('Ctrl Pts',(-1.39605031831591,23.8879210565933,2.19621137270406));
#10833=CARTESIAN_POINT('Ctrl Pts',(-1.98452338204,24.0962543899266,1.82214081731812));
#10834=CARTESIAN_POINT('Ctrl Pts',(-2.30712072697499,24.3045877232599,1.2039496816841));
#10835=CARTESIAN_POINT('Ctrl Pts',(-2.62971807190993,24.5129210565933,0.585758546050016));
#10836=CARTESIAN_POINT('Ctrl Pts',(-2.60000000000002,24.7212543899266,-0.110909354270829));
#10837=CARTESIAN_POINT('Ctrl Pts',(-2.57028192809006,24.92958772326,-0.807577254591853));
#10838=CARTESIAN_POINT('Ctrl Pts',(-2.19621137270413,25.1379210565933,-1.39605031831596));
#10839=CARTESIAN_POINT('Ctrl Pts',(-1.82214081731816,25.3462543899266,-1.98452338204004));
#10840=CARTESIAN_POINT('Ctrl Pts',(-1.20394968168413,25.5545877232599,-2.30712072697501));
#10841=CARTESIAN_POINT('Ctrl Pts',(-0.58575854605004,25.7629210565933,-2.6297180719101));
#10842=CARTESIAN_POINT('Ctrl Pts',(0.110909354270839,25.9712543899266,-2.6));
#10843=CARTESIAN_POINT('Ctrl Pts',(0.807577254591778,26.17958772326,-2.57028192809015));
#10844=CARTESIAN_POINT('Ctrl Pts',(1.39605031831587,26.3879210565933,-2.19621137270417));
#10845=CARTESIAN_POINT('Ctrl Pts',(1.98452338204001,26.5962543899266,-1.82214081731824));
#10846=CARTESIAN_POINT('Ctrl Pts',(2.30712072697495,26.80458772326,-1.2039496816842));
#10847=CARTESIAN_POINT('Ctrl Pts',(2.62971807190995,27.0129210565933,-0.585758546050172));
#10848=CARTESIAN_POINT('Ctrl Pts',(2.6,27.2212543899266,0.110909354270782));
#10849=CARTESIAN_POINT('Ctrl Pts',(2.57028192809007,27.42958772326,0.807577254591718));
#10850=CARTESIAN_POINT('Ctrl Pts',(2.19621137270409,27.6379210565932,1.39605031831588));
#10851=CARTESIAN_POINT('Ctrl Pts',(1.82214081731816,27.8462543899266,1.98452338203995));
#10852=CARTESIAN_POINT('Ctrl Pts',(1.20394968168409,28.05458772326,2.30712072697492));
#10853=CARTESIAN_POINT('Ctrl Pts',(0.585758546050084,28.2629210565933,2.62971807190984));
#10854=CARTESIAN_POINT('Ctrl Pts',(-0.11090935427086,28.4712543899266,2.59999999999994));
#10855=CARTESIAN_POINT('Ctrl Pts',(-0.807577254591778,28.67958772326,2.57028192809003));
#10856=CARTESIAN_POINT('Ctrl Pts',(-1.39605031831591,28.8879210565933,2.19621137270406));
#10857=CARTESIAN_POINT('Ctrl Pts',(-1.98452338204001,29.0962543899266,1.82214081731809));
#10858=CARTESIAN_POINT('Ctrl Pts',(-2.30712072697499,29.3045877232599,1.20394968168406));
#10859=CARTESIAN_POINT('Ctrl Pts',(-2.62971807190993,29.5129210565933,0.58575854605));
#10860=CARTESIAN_POINT('Ctrl Pts',(-2.60000000000002,29.7212543899266,-0.110909354270912));
#10861=CARTESIAN_POINT('Ctrl Pts',(-2.57028192809006,29.92958772326,-0.807577254591837));
#10862=CARTESIAN_POINT('Ctrl Pts',(-2.19621137270411,30.1379210565933,-1.39605031831594));
#10863=CARTESIAN_POINT('Ctrl Pts',(-1.82214081731815,30.3462543899266,-1.9845233820401));
#10864=CARTESIAN_POINT('Ctrl Pts',(-1.20394968168413,30.5545877232599,-2.307120726975));
#10865=CARTESIAN_POINT('Ctrl Pts',(-0.585758546050038,30.7629210565933,
-2.62971807191006));
#10866=CARTESIAN_POINT('Ctrl Pts',(0.110909354270839,30.9712543899266,-2.60000000000004));
#10867=CARTESIAN_POINT('Ctrl Pts',(0.807577254591778,31.17958772326,-2.57028192809014));
#10868=CARTESIAN_POINT('Ctrl Pts',(1.39605031831589,31.3879210565933,-2.19621137270416));
#10869=CARTESIAN_POINT('Ctrl Pts',(1.98452338204003,31.5962543899266,-1.82214081731823));
#10870=CARTESIAN_POINT('Ctrl Pts',(2.30712072697497,31.80458772326,-1.2039496816842));
#10871=CARTESIAN_POINT('Ctrl Pts',(2.62971807190996,32.0129210565933,-0.585758546050146));
#10872=CARTESIAN_POINT('Ctrl Pts',(2.59999999999998,32.2212543899266,0.110909354270782));
#10873=CARTESIAN_POINT('Ctrl Pts',(2.57028192809009,32.4295877232599,0.807577254591702));
#10874=CARTESIAN_POINT('Ctrl Pts',(2.19621137270409,32.6379210565933,1.39605031831587));
#10875=CARTESIAN_POINT('Ctrl Pts',(1.82214081731818,32.8462543899266,1.98452338203996));
#10876=CARTESIAN_POINT('Ctrl Pts',(1.20394968168411,33.05458772326,2.30712072697492));
#10877=CARTESIAN_POINT('Ctrl Pts',(0.585758546050062,33.2629210565933,2.62971807190987));
#10878=CARTESIAN_POINT('Ctrl Pts',(-0.11090935427086,33.4712543899266,2.59999999999995));
#10879=CARTESIAN_POINT('Ctrl Pts',(-0.807577254591756,33.67958772326,2.57028192809));
#10880=CARTESIAN_POINT('Ctrl Pts',(-1.39605031831591,33.8879210565933,2.19621137270406));
#10881=CARTESIAN_POINT('Ctrl Pts',(-1.98452338204,34.0962543899266,1.82214081731811));
#10882=CARTESIAN_POINT('Ctrl Pts',(-2.30712072697497,34.3045877232599,1.20394968168407));
#10883=CARTESIAN_POINT('Ctrl Pts',(-2.62971807190993,34.5129210565933,0.585758546050016));
#10884=CARTESIAN_POINT('Ctrl Pts',(-2.6,34.7212543899266,-0.110909354270923));
#10885=CARTESIAN_POINT('Ctrl Pts',(-2.57028192809006,34.92958772326,-0.807577254591853));
#10886=CARTESIAN_POINT('Ctrl Pts',(-2.19621137270411,35.1379210565933,-1.39605031831593));
#10887=CARTESIAN_POINT('Ctrl Pts',(-1.82214081731814,35.3462543899266,-1.98452338204009));
#10888=CARTESIAN_POINT('Ctrl Pts',(-1.20394968168411,35.55458772326,-2.30712072697501));
#10889=CARTESIAN_POINT('Ctrl Pts',(-0.58575854605004,35.7629210565933,-2.62971807190999));
#10890=CARTESIAN_POINT('Ctrl Pts',(0.110909354270858,35.9712543899266,-2.60000000000004));
#10891=CARTESIAN_POINT('Ctrl Pts',(0.807577254591799,36.17958772326,-2.57028192809016));
#10892=CARTESIAN_POINT('Ctrl Pts',(1.39605031831587,36.3879210565933,-2.19621137270416));
#10893=CARTESIAN_POINT('Ctrl Pts',(1.98452338204001,36.5962543899266,-1.82214081731826));
#10894=CARTESIAN_POINT('Ctrl Pts',(2.30712072697495,36.80458772326,-1.20394968168412));
#10895=CARTESIAN_POINT('Ctrl Pts',(2.62971807190995,37.0129210565933,-0.585758546050162));
#10896=CARTESIAN_POINT('Ctrl Pts',(2.6,37.2212543899266,0.110909354270793));
#10897=CARTESIAN_POINT('Ctrl Pts',(2.57028192809009,37.42958772326,0.807577254591713));
#10898=CARTESIAN_POINT('Ctrl Pts',(2.19621137270409,37.6379210565933,1.39605031831585));
#10899=CARTESIAN_POINT('Ctrl Pts',(1.82214081731818,37.8462543899266,1.98452338203995));
#10900=CARTESIAN_POINT('Ctrl Pts',(1.20394968168411,38.05458772326,2.30712072697493));
#10901=CARTESIAN_POINT('Ctrl Pts',(0.585758546050084,38.2629210565933,2.62971807190984));
#10902=CARTESIAN_POINT('Ctrl Pts',(-0.110909354270881,38.4712543899266,
2.59999999999996));
#10903=CARTESIAN_POINT('Ctrl Pts',(-0.807577254591756,38.67958772326,2.57028192809004));
#10904=CARTESIAN_POINT('Ctrl Pts',(-1.39605031831591,38.8879210565933,2.19621137270406));
#10905=CARTESIAN_POINT('Ctrl Pts',(-1.98452338204001,39.0962543899267,1.82214081731809));
#10906=CARTESIAN_POINT('Ctrl Pts',(-2.30712072697501,39.30458772326,1.20394968168406));
#10907=CARTESIAN_POINT('Ctrl Pts',(-2.62971807190992,39.5129210565933,0.585758546049984));
#10908=CARTESIAN_POINT('Ctrl Pts',(-2.60000000000002,39.7212543899267,-0.110909354270912));
#10909=CARTESIAN_POINT('Ctrl Pts',(-2.60000000000002,0.278745610073436,
0.110909354270912));
#10910=CARTESIAN_POINT('Ctrl Pts',(-2.62971807190994,0.487078943406783,
-0.585758546050092));
#10911=CARTESIAN_POINT('Ctrl Pts',(-2.307120726975,0.695412276740106,-1.20394968168414));
#10912=CARTESIAN_POINT('Ctrl Pts',(-1.98452338204005,0.903745610073436,
-1.82214081731813));
#10913=CARTESIAN_POINT('Ctrl Pts',(-1.39605031831596,1.11207894340677,-2.19621137270408));
#10914=CARTESIAN_POINT('Ctrl Pts',(-0.807577254591829,1.32041227674011,
-2.57028192809019));
#10915=CARTESIAN_POINT('Ctrl Pts',(-0.110909354270912,1.52874561007344,
-2.60000000000008));
#10916=CARTESIAN_POINT('Ctrl Pts',(0.585758546050027,1.73707894340677,-2.62971807191004));
#10917=CARTESIAN_POINT('Ctrl Pts',(1.20394968168406,1.9454122767401,-2.30712072697508));
#10918=CARTESIAN_POINT('Ctrl Pts',(1.82214081731812,2.15374561007341,-1.98452338204012));
#10919=CARTESIAN_POINT('Ctrl Pts',(2.19621137270406,2.36207894340677,-1.39605031831594));
#10920=CARTESIAN_POINT('Ctrl Pts',(2.57028192809005,2.5704122767401,-0.807577254591869));
#10921=CARTESIAN_POINT('Ctrl Pts',(2.59999999999998,2.77874561007344,-0.110909354270907));
#10922=CARTESIAN_POINT('Ctrl Pts',(2.62971807190997,2.98707894340676,0.585758546049919));
#10923=CARTESIAN_POINT('Ctrl Pts',(2.30712072697498,3.19541227674011,1.20394968168406));
#10924=CARTESIAN_POINT('Ctrl Pts',(1.98452338204005,3.40374561007341,1.82214081731804));
#10925=CARTESIAN_POINT('Ctrl Pts',(1.39605031831592,3.61207894340678,2.19621137270405));
#10926=CARTESIAN_POINT('Ctrl Pts',(0.807577254591831,3.82041227674012,2.57028192808996));
#10927=CARTESIAN_POINT('Ctrl Pts',(0.110909354270912,4.02874561007344,2.6));
#10928=CARTESIAN_POINT('Ctrl Pts',(-0.585758546050005,4.23707894340677,
2.62971807190995));
#10929=CARTESIAN_POINT('Ctrl Pts',(-1.20394968168408,4.4454122767401,2.30712072697499));
#10930=CARTESIAN_POINT('Ctrl Pts',(-1.8221408173181,4.65374561007344,1.98452338203996));
#10931=CARTESIAN_POINT('Ctrl Pts',(-2.19621137270408,4.86207894340675,1.39605031831586));
#10932=CARTESIAN_POINT('Ctrl Pts',(-2.57028192809003,5.07041227674009,0.807577254591729));
#10933=CARTESIAN_POINT('Ctrl Pts',(-2.60000000000002,5.27874561007344,0.110909354270912));
#10934=CARTESIAN_POINT('Ctrl Pts',(-2.62971807190994,5.48707894340677,-0.585758546050172));
#10935=CARTESIAN_POINT('Ctrl Pts',(-2.30712072697502,5.69541227674011,-1.20394968168414));
#10936=CARTESIAN_POINT('Ctrl Pts',(-1.98452338204004,5.90374561007343,-1.82214081731821));
#10937=CARTESIAN_POINT('Ctrl Pts',(-1.39605031831596,6.11207894340677,-2.19621137270408));
#10938=CARTESIAN_POINT('Ctrl Pts',(-0.80757725459181,6.32041227674011,-2.57028192809014));
#10939=CARTESIAN_POINT('Ctrl Pts',(-0.110909354270912,6.52874561007346,
-2.60000000000008));
#10940=CARTESIAN_POINT('Ctrl Pts',(0.585758546050008,6.73707894340677,-2.62971807191004));
#10941=CARTESIAN_POINT('Ctrl Pts',(1.20394968168404,6.94541227674013,-2.30712072697508));
#10942=CARTESIAN_POINT('Ctrl Pts',(1.82214081731814,7.15374561007344,-1.98452338204004));
#10943=CARTESIAN_POINT('Ctrl Pts',(2.19621137270408,7.36207894340678,-1.39605031831594));
#10944=CARTESIAN_POINT('Ctrl Pts',(2.57028192809007,7.57041227674014,-0.807577254591929));
#10945=CARTESIAN_POINT('Ctrl Pts',(2.6,7.77874561007344,-0.110909354270907));
#10946=CARTESIAN_POINT('Ctrl Pts',(2.62971807190995,7.98707894340679,0.585758546049914));
#10947=CARTESIAN_POINT('Ctrl Pts',(2.30712072697498,8.19541227674011,1.20394968168406));
#10948=CARTESIAN_POINT('Ctrl Pts',(1.98452338204007,8.40374561007345,1.82214081731803));
#10949=CARTESIAN_POINT('Ctrl Pts',(1.39605031831592,8.6120789434068,2.19621137270408));
#10950=CARTESIAN_POINT('Ctrl Pts',(0.807577254591834,8.82041227674012,2.57028192808996));
#10951=CARTESIAN_POINT('Ctrl Pts',(0.110909354270891,9.02874561007344,2.59999999999996));
#10952=CARTESIAN_POINT('Ctrl Pts',(-0.585758546050005,9.2370789434068,2.6297180719099));
#10953=CARTESIAN_POINT('Ctrl Pts',(-1.20394968168408,9.44541227674011,2.30712072697499));
#10954=CARTESIAN_POINT('Ctrl Pts',(-1.8221408173181,9.65374561007347,1.98452338203995));
#10955=CARTESIAN_POINT('Ctrl Pts',(-2.1962113727041,9.8620789434068,1.39605031831586));
#10956=CARTESIAN_POINT('Ctrl Pts',(-2.57028192809005,10.0704122767401,0.807577254591745));
#10957=CARTESIAN_POINT('Ctrl Pts',(-2.6,10.2787456100734,0.110909354270912));
#10958=CARTESIAN_POINT('Ctrl Pts',(-2.62971807190994,10.4870789434068,-0.585758546050097));
#10959=CARTESIAN_POINT('Ctrl Pts',(-2.30712072697502,10.6954122767401,-1.20394968168415));
#10960=CARTESIAN_POINT('Ctrl Pts',(-1.98452338204002,10.9037456100735,-1.82214081731821));
#10961=CARTESIAN_POINT('Ctrl Pts',(-1.39605031831596,11.1120789434068,-2.19621137270408));
#10962=CARTESIAN_POINT('Ctrl Pts',(-0.807577254591831,11.3204122767401,
-2.57028192809014));
#10963=CARTESIAN_POINT('Ctrl Pts',(-0.110909354270912,11.5287456100735,
-2.60000000000007));
#10964=CARTESIAN_POINT('Ctrl Pts',(0.585758546050027,11.7370789434068,-2.62971807191004));
#10965=CARTESIAN_POINT('Ctrl Pts',(1.20394968168406,11.9454122767401,-2.30712072697508));
#10966=CARTESIAN_POINT('Ctrl Pts',(1.82214081731812,12.1537456100735,-1.98452338204013));
#10967=CARTESIAN_POINT('Ctrl Pts',(2.19621137270406,12.3620789434068,-1.39605031831594));
#10968=CARTESIAN_POINT('Ctrl Pts',(2.57028192809007,12.5704122767401,-0.807577254591923));
#10969=CARTESIAN_POINT('Ctrl Pts',(2.6,12.7787456100734,-0.110909354270907));
#10970=CARTESIAN_POINT('Ctrl Pts',(2.62971807190997,12.9870789434068,0.585758546049914));
#10971=CARTESIAN_POINT('Ctrl Pts',(2.30712072697498,13.1954122767401,1.20394968168406));
#10972=CARTESIAN_POINT('Ctrl Pts',(1.98452338204005,13.4037456100734,1.82214081731803));
#10973=CARTESIAN_POINT('Ctrl Pts',(1.39605031831592,13.6120789434068,2.19621137270407));
#10974=CARTESIAN_POINT('Ctrl Pts',(0.807577254591831,13.8204122767401,2.57028192808997));
#10975=CARTESIAN_POINT('Ctrl Pts',(0.110909354270912,14.0287456100735,2.59999999999999));
#10976=CARTESIAN_POINT('Ctrl Pts',(-0.585758546049984,14.2370789434068,
2.62971807190992));
#10977=CARTESIAN_POINT('Ctrl Pts',(-1.20394968168406,14.4454122767402,2.30712072697499));
#10978=CARTESIAN_POINT('Ctrl Pts',(-1.82214081731812,14.6537456100735,1.98452338203996));
#10979=CARTESIAN_POINT('Ctrl Pts',(-2.19621137270408,14.8620789434068,1.39605031831585));
#10980=CARTESIAN_POINT('Ctrl Pts',(-2.57028192809005,15.0704122767401,0.807577254591761));
#10981=CARTESIAN_POINT('Ctrl Pts',(-2.6,15.2787456100734,0.110909354270912));
#10982=CARTESIAN_POINT('Ctrl Pts',(-2.62971807190993,15.4870789434068,-0.585758546050097));
#10983=CARTESIAN_POINT('Ctrl Pts',(-2.307120726975,15.6954122767401,-1.20394968168414));
#10984=CARTESIAN_POINT('Ctrl Pts',(-1.98452338204004,15.9037456100734,-1.82214081731821));
#10985=CARTESIAN_POINT('Ctrl Pts',(-1.39605031831596,16.1120789434068,-2.19621137270408));
#10986=CARTESIAN_POINT('Ctrl Pts',(-0.80757725459181,16.3204122767401,-2.5702819280902));
#10987=CARTESIAN_POINT('Ctrl Pts',(-0.110909354270912,16.5287456100734,
-2.60000000000008));
#10988=CARTESIAN_POINT('Ctrl Pts',(0.58575854605003,16.7370789434068,-2.62971807191002));
#10989=CARTESIAN_POINT('Ctrl Pts',(1.20394968168404,16.9454122767401,-2.30712072697508));
#10990=CARTESIAN_POINT('Ctrl Pts',(1.82214081731814,17.1537456100735,-1.98452338204012));
#10991=CARTESIAN_POINT('Ctrl Pts',(2.19621137270406,17.3620789434068,-1.39605031831595));
#10992=CARTESIAN_POINT('Ctrl Pts',(2.57028192809007,17.5704122767402,-0.80757725459188));
#10993=CARTESIAN_POINT('Ctrl Pts',(2.59999999999998,17.7787456100734,-0.110909354270907));
#10994=CARTESIAN_POINT('Ctrl Pts',(2.62971807190997,17.9870789434068,0.585758546049935));
#10995=CARTESIAN_POINT('Ctrl Pts',(2.30712072697498,18.1954122767402,1.20394968168405));
#10996=CARTESIAN_POINT('Ctrl Pts',(1.98452338204005,18.4037456100735,1.82214081731802));
#10997=CARTESIAN_POINT('Ctrl Pts',(1.39605031831592,18.6120789434068,2.19621137270408));
#10998=CARTESIAN_POINT('Ctrl Pts',(0.807577254591834,18.8204122767402,2.57028192808997));
#10999=CARTESIAN_POINT('Ctrl Pts',(0.110909354270891,19.0287456100735,2.59999999999999));
#11000=CARTESIAN_POINT('Ctrl Pts',(-0.585758546050005,19.2370789434068,
2.62971807190989));
#11001=CARTESIAN_POINT('Ctrl Pts',(-1.20394968168408,19.4454122767402,2.30712072697499));
#11002=CARTESIAN_POINT('Ctrl Pts',(-1.82214081731812,19.6537456100735,1.98452338203994));
#11003=CARTESIAN_POINT('Ctrl Pts',(-2.1962113727041,19.8620789434068,1.39605031831591));
#11004=CARTESIAN_POINT('Ctrl Pts',(-2.57028192809004,20.0704122767402,0.807577254591761));
#11005=CARTESIAN_POINT('Ctrl Pts',(-2.6,20.2787456100735,0.110909354270902));
#11006=CARTESIAN_POINT('Ctrl Pts',(-2.62971807190994,20.4870789434068,-0.585758546050065));
#11007=CARTESIAN_POINT('Ctrl Pts',(-2.30712072697502,20.6954122767402,-1.20394968168415));
#11008=CARTESIAN_POINT('Ctrl Pts',(-1.98452338204004,20.9037456100735,-1.82214081731816));
#11009=CARTESIAN_POINT('Ctrl Pts',(-1.39605031831594,21.1120789434068,-2.19621137270408));
#11010=CARTESIAN_POINT('Ctrl Pts',(-0.807577254591831,21.3204122767402,
-2.57028192809015));
#11011=CARTESIAN_POINT('Ctrl Pts',(-0.110909354270933,21.5287456100735,
-2.60000000000005));
#11012=CARTESIAN_POINT('Ctrl Pts',(0.585758546050027,21.7370789434068,-2.62971807191006));
#11013=CARTESIAN_POINT('Ctrl Pts',(1.20394968168404,21.9454122767401,-2.30712072697508));
#11014=CARTESIAN_POINT('Ctrl Pts',(1.82214081731812,22.1537456100735,-1.98452338204008));
#11015=CARTESIAN_POINT('Ctrl Pts',(2.19621137270406,22.3620789434068,-1.39605031831599));
#11016=CARTESIAN_POINT('Ctrl Pts',(2.57028192809005,22.5704122767402,-0.807577254591907));
#11017=CARTESIAN_POINT('Ctrl Pts',(2.6,22.7787456100735,-0.110909354270912));
#11018=CARTESIAN_POINT('Ctrl Pts',(2.62971807190995,22.9870789434068,0.585758546049909));
#11019=CARTESIAN_POINT('Ctrl Pts',(2.30712072697499,23.1954122767402,1.20394968168404));
#11020=CARTESIAN_POINT('Ctrl Pts',(1.98452338204007,23.4037456100735,1.82214081731806));
#11021=CARTESIAN_POINT('Ctrl Pts',(1.39605031831592,23.6120789434068,2.19621137270408));
#11022=CARTESIAN_POINT('Ctrl Pts',(0.807577254591853,23.8204122767402,2.57028192808998));
#11023=CARTESIAN_POINT('Ctrl Pts',(0.110909354270891,24.0287456100735,2.59999999999999));
#11024=CARTESIAN_POINT('Ctrl Pts',(-0.585758546049984,24.2370789434068,
2.62971807190988));
#11025=CARTESIAN_POINT('Ctrl Pts',(-1.20394968168408,24.4454122767401,2.307120726975));
#11026=CARTESIAN_POINT('Ctrl Pts',(-1.82214081731811,24.6537456100735,1.98452338203996));
#11027=CARTESIAN_POINT('Ctrl Pts',(-2.19621137270408,24.8620789434068,1.39605031831592));
#11028=CARTESIAN_POINT('Ctrl Pts',(-2.57028192809004,25.0704122767402,0.807577254591788));
#11029=CARTESIAN_POINT('Ctrl Pts',(-2.6,25.2787456100735,0.110909354270902));
#11030=CARTESIAN_POINT('Ctrl Pts',(-2.62971807190995,25.4870789434068,-0.585758546050065));
#11031=CARTESIAN_POINT('Ctrl Pts',(-2.307120726975,25.6954122767402,-1.20394968168412));
#11032=CARTESIAN_POINT('Ctrl Pts',(-1.98452338204004,25.9037456100735,-1.82214081731821));
#11033=CARTESIAN_POINT('Ctrl Pts',(-1.39605031831596,26.1120789434069,-2.19621137270412));
#11034=CARTESIAN_POINT('Ctrl Pts',(-0.807577254591831,26.3204122767401,
-2.57028192809014));
#11035=CARTESIAN_POINT('Ctrl Pts',(-0.110909354270912,26.5287456100735,
-2.60000000000005));
#11036=CARTESIAN_POINT('Ctrl Pts',(0.585758546050008,26.7370789434069,-2.62971807191005));
#11037=CARTESIAN_POINT('Ctrl Pts',(1.20394968168406,26.9454122767402,-2.30712072697512));
#11038=CARTESIAN_POINT('Ctrl Pts',(1.82214081731812,27.1537456100735,-1.98452338204008));
#11039=CARTESIAN_POINT('Ctrl Pts',(2.19621137270408,27.3620789434068,-1.39605031831603));
#11040=CARTESIAN_POINT('Ctrl Pts',(2.57028192809005,27.5704122767402,-0.807577254591918));
#11041=CARTESIAN_POINT('Ctrl Pts',(2.59999999999998,27.7787456100735,-0.110909354271001));
#11042=CARTESIAN_POINT('Ctrl Pts',(2.62971807190995,27.9870789434069,0.585758546049935));
#11043=CARTESIAN_POINT('Ctrl Pts',(2.30712072697499,28.1954122767402,1.20394968168403));
#11044=CARTESIAN_POINT('Ctrl Pts',(1.98452338204005,28.4037456100735,1.82214081731803));
#11045=CARTESIAN_POINT('Ctrl Pts',(1.39605031831592,28.6120789434068,2.19621137270408));
#11046=CARTESIAN_POINT('Ctrl Pts',(0.807577254591834,28.8204122767402,2.57028192808996));
#11047=CARTESIAN_POINT('Ctrl Pts',(0.110909354270912,29.0287456100734,2.59999999999999));
#11048=CARTESIAN_POINT('Ctrl Pts',(-0.585758546050005,29.2370789434068,
2.6297180719099));
#11049=CARTESIAN_POINT('Ctrl Pts',(-1.20394968168408,29.4454122767402,2.307120726975));
#11050=CARTESIAN_POINT('Ctrl Pts',(-1.82214081731812,29.6537456100735,1.98452338203995));
#11051=CARTESIAN_POINT('Ctrl Pts',(-2.19621137270408,29.8620789434069,1.39605031831591));
#11052=CARTESIAN_POINT('Ctrl Pts',(-2.57028192809004,30.0704122767402,0.807577254591761));
#11053=CARTESIAN_POINT('Ctrl Pts',(-2.6,30.2787456100735,0.110909354270865));
#11054=CARTESIAN_POINT('Ctrl Pts',(-2.62971807190995,30.4870789434069,-0.58575854605007));
#11055=CARTESIAN_POINT('Ctrl Pts',(-2.30712072697502,30.6954122767402,-1.20394968168412));
#11056=CARTESIAN_POINT('Ctrl Pts',(-1.98452338204004,30.9037456100735,-1.82214081731818));
#11057=CARTESIAN_POINT('Ctrl Pts',(-1.39605031831594,31.1120789434069,-2.19621137270412));
#11058=CARTESIAN_POINT('Ctrl Pts',(-0.807577254591831,31.3204122767402,
-2.57028192809019));
#11059=CARTESIAN_POINT('Ctrl Pts',(-0.110909354270912,31.5287456100735,
-2.60000000000006));
#11060=CARTESIAN_POINT('Ctrl Pts',(0.585758546050008,31.7370789434068,-2.62971807191004));
#11061=CARTESIAN_POINT('Ctrl Pts',(1.20394968168404,31.9454122767402,-2.30712072697511));
#11062=CARTESIAN_POINT('Ctrl Pts',(1.82214081731812,32.1537456100735,-1.98452338204011));
#11063=CARTESIAN_POINT('Ctrl Pts',(2.19621137270404,32.3620789434068,-1.39605031831603));
#11064=CARTESIAN_POINT('Ctrl Pts',(2.57028192809005,32.5704122767402,-0.807577254591907));
#11065=CARTESIAN_POINT('Ctrl Pts',(2.6,32.7787456100735,-0.110909354270959));
#11066=CARTESIAN_POINT('Ctrl Pts',(2.62971807190995,32.9870789434069,0.585758546049903));
#11067=CARTESIAN_POINT('Ctrl Pts',(2.30712072697499,33.1954122767402,1.20394968168402));
#11068=CARTESIAN_POINT('Ctrl Pts',(1.98452338204004,33.4037456100735,1.82214081731806));
#11069=CARTESIAN_POINT('Ctrl Pts',(1.39605031831594,33.6120789434069,2.19621137270407));
#11070=CARTESIAN_POINT('Ctrl Pts',(0.807577254591853,33.8204122767402,2.57028192808998));
#11071=CARTESIAN_POINT('Ctrl Pts',(0.110909354270891,34.0287456100735,2.59999999999999));
#11072=CARTESIAN_POINT('Ctrl Pts',(-0.585758546050008,34.2370789434069,
2.62971807190989));
#11073=CARTESIAN_POINT('Ctrl Pts',(-1.20394968168408,34.4454122767402,2.30712072697499));
#11074=CARTESIAN_POINT('Ctrl Pts',(-1.82214081731812,34.6537456100735,1.98452338203996));
#11075=CARTESIAN_POINT('Ctrl Pts',(-2.1962113727041,34.8620789434069,1.39605031831591));
#11076=CARTESIAN_POINT('Ctrl Pts',(-2.57028192809004,35.0704122767402,0.807577254591772));
#11077=CARTESIAN_POINT('Ctrl Pts',(-2.6,35.2787456100735,0.110909354270876));
#11078=CARTESIAN_POINT('Ctrl Pts',(-2.62971807190993,35.4870789434068,-0.585758546050086));
#11079=CARTESIAN_POINT('Ctrl Pts',(-2.30712072697501,35.6954122767402,-1.20394968168413));
#11080=CARTESIAN_POINT('Ctrl Pts',(-1.98452338204002,35.9037456100735,-1.82214081731821));
#11081=CARTESIAN_POINT('Ctrl Pts',(-1.39605031831594,36.1120789434069,-2.19621137270412));
#11082=CARTESIAN_POINT('Ctrl Pts',(-0.80757725459181,36.3204122767402,-2.57028192809015));
#11083=CARTESIAN_POINT('Ctrl Pts',(-0.110909354270933,36.5287456100735,
-2.60000000000005));
#11084=CARTESIAN_POINT('Ctrl Pts',(0.585758546050008,36.7370789434069,-2.62971807191005));
#11085=CARTESIAN_POINT('Ctrl Pts',(1.20394968168406,36.9454122767402,-2.3071207269751));
#11086=CARTESIAN_POINT('Ctrl Pts',(1.82214081731814,37.1537456100735,-1.9845233820401));
#11087=CARTESIAN_POINT('Ctrl Pts',(2.19621137270408,37.3620789434068,-1.39605031831602));
#11088=CARTESIAN_POINT('Ctrl Pts',(2.57028192809005,37.5704122767402,-0.807577254591923));
#11089=CARTESIAN_POINT('Ctrl Pts',(2.6,37.7787456100735,-0.110909354270975));
#11090=CARTESIAN_POINT('Ctrl Pts',(2.62971807190995,37.9870789434069,0.585758546049941));
#11091=CARTESIAN_POINT('Ctrl Pts',(2.307120726975,38.1954122767402,1.20394968168401));
#11092=CARTESIAN_POINT('Ctrl Pts',(1.98452338204005,38.4037456100735,1.82214081731804));
#11093=CARTESIAN_POINT('Ctrl Pts',(1.39605031831594,38.6120789434069,2.19621137270407));
#11094=CARTESIAN_POINT('Ctrl Pts',(0.807577254591853,38.8204122767402,2.57028192808997));
#11095=CARTESIAN_POINT('Ctrl Pts',(0.110909354270891,39.0287456100735,2.59999999999999));
#11096=CARTESIAN_POINT('Ctrl Pts',(-0.585758546050005,39.2370789434069,
2.6297180719099));
#11097=CARTESIAN_POINT('Ctrl Pts',(-1.20394968168408,39.4454122767402,2.30712072697499));
#11098=CARTESIAN_POINT('Ctrl Pts',(-1.8221408173181,39.6537456100736,1.98452338203994));
#11099=CARTESIAN_POINT('Ctrl Pts',(-2.19621137270408,39.8620789434069,1.39605031831592));
#11100=CARTESIAN_POINT('Ctrl Pts',(-2.57028192809004,40.0704122767402,0.807577254591751));
#11101=CARTESIAN_POINT('Ctrl Pts',(-2.6,40.2787456100736,0.110909354270871));
#11102=CARTESIAN_POINT('Ctrl Pts',(-2.,0.278745610073468,0.110909354270813));
#11103=CARTESIAN_POINT('Ctrl Pts',(-2.02971807190995,0.487078943406699,
-0.424989030591362));
#11104=CARTESIAN_POINT('Ctrl Pts',(-1.78750548470433,0.695412276740089,
-0.90394968168412));
#11105=CARTESIAN_POINT('Ctrl Pts',(-1.54529289749872,0.903745610073333,
-1.3829103327768));
#11106=CARTESIAN_POINT('Ctrl Pts',(-1.09605031831593,1.11207894340676,-1.67659613043348));
#11107=CARTESIAN_POINT('Ctrl Pts',(-0.646807739133152,1.32041227674011,
-1.97028192809006));
#11108=CARTESIAN_POINT('Ctrl Pts',(-0.110909354270893,1.52874561007344,
-2.00000000000001));
#11109=CARTESIAN_POINT('Ctrl Pts',(0.42498903059134,1.7370789434067,-2.02971807190998));
#11110=CARTESIAN_POINT('Ctrl Pts',(0.903949681684066,1.94541227674011,-1.78750548470433));
#11111=CARTESIAN_POINT('Ctrl Pts',(1.38291033277679,2.15374561007344,-1.54529289749872));
#11112=CARTESIAN_POINT('Ctrl Pts',(1.67659613043343,2.36207894340677,-1.09605031831594));
#11113=CARTESIAN_POINT('Ctrl Pts',(1.97028192809005,2.57041227674009,-0.646807739133166));
#11114=CARTESIAN_POINT('Ctrl Pts',(2.00000000000003,2.77874561007344,-0.110909354270911));
#11115=CARTESIAN_POINT('Ctrl Pts',(2.02971807190995,2.98707894340676,0.424989030591319));
#11116=CARTESIAN_POINT('Ctrl Pts',(1.78750548470433,3.1954122767401,0.903949681684016));
#11117=CARTESIAN_POINT('Ctrl Pts',(1.54529289749872,3.40374561007338,1.38291033277678));
#11118=CARTESIAN_POINT('Ctrl Pts',(1.09605031831593,3.61207894340677,1.67659613043342));
#11119=CARTESIAN_POINT('Ctrl Pts',(0.646807739133154,3.82041227674006,1.97028192809004));
#11120=CARTESIAN_POINT('Ctrl Pts',(0.110909354270907,4.02874561007344,1.99999999999995));
#11121=CARTESIAN_POINT('Ctrl Pts',(-0.424989030591324,4.23707894340672,
2.02971807190993));
#11122=CARTESIAN_POINT('Ctrl Pts',(-0.903949681684066,4.44541227674011,
1.78750548470433));
#11123=CARTESIAN_POINT('Ctrl Pts',(-1.38291033277679,4.65374561007344,1.54529289749866));
#11124=CARTESIAN_POINT('Ctrl Pts',(-1.67659613043344,4.8620789434068,1.09605031831587));
#11125=CARTESIAN_POINT('Ctrl Pts',(-1.97028192809005,5.07041227674005,0.646807739133138));
#11126=CARTESIAN_POINT('Ctrl Pts',(-2.,5.27874561007342,0.110909354270813));
#11127=CARTESIAN_POINT('Ctrl Pts',(-2.02971807190995,5.48707894340671,-0.424989030591405));
#11128=CARTESIAN_POINT('Ctrl Pts',(-1.78750548470433,5.6954122767401,-0.90394968168412));
#11129=CARTESIAN_POINT('Ctrl Pts',(-1.54529289749872,5.90374561007338,-1.38291033277678));
#11130=CARTESIAN_POINT('Ctrl Pts',(-1.09605031831592,6.11207894340678,-1.67659613043342));
#11131=CARTESIAN_POINT('Ctrl Pts',(-0.646807739133139,6.3204122767401,-1.97028192809006));
#11132=CARTESIAN_POINT('Ctrl Pts',(-0.110909354270905,6.52874561007347,
-2.00000000000006));
#11133=CARTESIAN_POINT('Ctrl Pts',(0.424989030591338,6.73707894340672,-2.02971807190996));
#11134=CARTESIAN_POINT('Ctrl Pts',(0.903949681684068,6.94541227674014,-1.78750548470433));
#11135=CARTESIAN_POINT('Ctrl Pts',(1.38291033277681,7.15374561007342,-1.54529289749877));
#11136=CARTESIAN_POINT('Ctrl Pts',(1.6765961304334,7.36207894340677,-1.09605031831599));
#11137=CARTESIAN_POINT('Ctrl Pts',(1.97028192809006,7.57041227674011,-0.646807739133152));
#11138=CARTESIAN_POINT('Ctrl Pts',(2.,7.77874561007349,-0.110909354270917));
#11139=CARTESIAN_POINT('Ctrl Pts',(2.02971807190995,7.98707894340672,0.424989030591319));
#11140=CARTESIAN_POINT('Ctrl Pts',(1.78750548470433,8.19541227674012,0.903949681684058));
#11141=CARTESIAN_POINT('Ctrl Pts',(1.54529289749873,8.40374561007341,1.3829103327768));
#11142=CARTESIAN_POINT('Ctrl Pts',(1.09605031831593,8.6120789434068,1.67659613043337));
#11143=CARTESIAN_POINT('Ctrl Pts',(0.646807739133154,8.82041227674011,1.97028192809005));
#11144=CARTESIAN_POINT('Ctrl Pts',(0.110909354270904,9.02874561007346,1.99999999999994));
#11145=CARTESIAN_POINT('Ctrl Pts',(-0.424989030591337,9.23707894340678,
2.02971807190995));
#11146=CARTESIAN_POINT('Ctrl Pts',(-0.903949681684064,9.44541227674011,
1.78750548470427));
#11147=CARTESIAN_POINT('Ctrl Pts',(-1.38291033277679,9.65374561007344,1.54529289749871));
#11148=CARTESIAN_POINT('Ctrl Pts',(-1.67659613043342,9.86207894340678,1.09605031831593));
#11149=CARTESIAN_POINT('Ctrl Pts',(-1.97028192809005,10.0704122767401,0.646807739133152));
#11150=CARTESIAN_POINT('Ctrl Pts',(-1.99999999999999,10.2787456100735,0.110909354270841));
#11151=CARTESIAN_POINT('Ctrl Pts',(-2.02971807190994,10.4870789434068,-0.42498903059134));
#11152=CARTESIAN_POINT('Ctrl Pts',(-1.78750548470433,10.6954122767401,-0.903949681684169));
#11153=CARTESIAN_POINT('Ctrl Pts',(-1.54529289749871,10.9037456100734,-1.38291033277681));
#11154=CARTESIAN_POINT('Ctrl Pts',(-1.09605031831593,11.1120789434068,-1.67659613043348));
#11155=CARTESIAN_POINT('Ctrl Pts',(-0.646807739133152,11.3204122767401,
-1.97028192809006));
#11156=CARTESIAN_POINT('Ctrl Pts',(-0.110909354270907,11.5287456100735,
-2.00000000000002));
#11157=CARTESIAN_POINT('Ctrl Pts',(0.424989030591338,11.7370789434068,-2.02971807190997));
#11158=CARTESIAN_POINT('Ctrl Pts',(0.903949681684066,11.9454122767401,-1.78750548470433));
#11159=CARTESIAN_POINT('Ctrl Pts',(1.3829103327768,12.1537456100734,-1.54529289749877));
#11160=CARTESIAN_POINT('Ctrl Pts',(1.67659613043342,12.3620789434068,-1.09605031831594));
#11161=CARTESIAN_POINT('Ctrl Pts',(1.97028192809008,12.5704122767401,-0.646807739133166));
#11162=CARTESIAN_POINT('Ctrl Pts',(2.,12.7787456100735,-0.110909354270959));
#11163=CARTESIAN_POINT('Ctrl Pts',(2.02971807190995,12.9870789434068,0.42498903059134));
#11164=CARTESIAN_POINT('Ctrl Pts',(1.78750548470433,13.1954122767401,0.903949681684009));
#11165=CARTESIAN_POINT('Ctrl Pts',(1.54529289749872,13.4037456100734,1.38291033277679));
#11166=CARTESIAN_POINT('Ctrl Pts',(1.09605031831593,13.6120789434068,1.67659613043342));
#11167=CARTESIAN_POINT('Ctrl Pts',(0.646807739133154,13.8204122767401,1.97028192809006));
#11168=CARTESIAN_POINT('Ctrl Pts',(0.110909354270907,14.0287456100735,1.99999999999997));
#11169=CARTESIAN_POINT('Ctrl Pts',(-0.424989030591338,14.2370789434068,
2.02971807190995));
#11170=CARTESIAN_POINT('Ctrl Pts',(-0.903949681684066,14.4454122767402,
1.78750548470424));
#11171=CARTESIAN_POINT('Ctrl Pts',(-1.38291033277679,14.6537456100734,1.54529289749866));
#11172=CARTESIAN_POINT('Ctrl Pts',(-1.67659613043342,14.8620789434068,1.09605031831587));
#11173=CARTESIAN_POINT('Ctrl Pts',(-1.97028192809004,15.0704122767401,0.646807739133166));
#11174=CARTESIAN_POINT('Ctrl Pts',(-2.,15.2787456100735,0.110909354270848));
#11175=CARTESIAN_POINT('Ctrl Pts',(-2.02971807190995,15.4870789434068,-0.424989030591448));
#11176=CARTESIAN_POINT('Ctrl Pts',(-1.78750548470433,15.6954122767401,-0.903949681684079));
#11177=CARTESIAN_POINT('Ctrl Pts',(-1.54529289749872,15.9037456100734,-1.3829103327768));
#11178=CARTESIAN_POINT('Ctrl Pts',(-1.09605031831592,16.1120789434068,-1.67659613043346));
#11179=CARTESIAN_POINT('Ctrl Pts',(-0.646807739133152,16.3204122767401,
-1.97028192809011));
#11180=CARTESIAN_POINT('Ctrl Pts',(-0.110909354270907,16.5287456100735,
-2.00000000000005));
#11181=CARTESIAN_POINT('Ctrl Pts',(0.42498903059134,16.7370789434068,-2.02971807190995));
#11182=CARTESIAN_POINT('Ctrl Pts',(0.90394968168408,16.9454122767401,-1.78750548470433));
#11183=CARTESIAN_POINT('Ctrl Pts',(1.38291033277679,17.1537456100734,-1.54529289749872));
#11184=CARTESIAN_POINT('Ctrl Pts',(1.67659613043342,17.3620789434068,-1.09605031831599));
#11185=CARTESIAN_POINT('Ctrl Pts',(1.97028192809005,17.5704122767401,-0.646807739133152));
#11186=CARTESIAN_POINT('Ctrl Pts',(2.,17.7787456100735,-0.110909354270917));
#11187=CARTESIAN_POINT('Ctrl Pts',(2.02971807190995,17.9870789434068,0.424989030591283));
#11188=CARTESIAN_POINT('Ctrl Pts',(1.78750548470433,18.1954122767401,0.903949681684051));
#11189=CARTESIAN_POINT('Ctrl Pts',(1.54529289749873,18.4037456100734,1.3829103327768));
#11190=CARTESIAN_POINT('Ctrl Pts',(1.09605031831593,18.6120789434068,1.67659613043337));
#11191=CARTESIAN_POINT('Ctrl Pts',(0.646807739133154,18.8204122767401,1.97028192809005));
#11192=CARTESIAN_POINT('Ctrl Pts',(0.110909354270905,19.0287456100735,1.99999999999995));
#11193=CARTESIAN_POINT('Ctrl Pts',(-0.424989030591338,19.2370789434068,
2.02971807190995));
#11194=CARTESIAN_POINT('Ctrl Pts',(-0.903949681684064,19.4454122767402,
1.78750548470426));
#11195=CARTESIAN_POINT('Ctrl Pts',(-1.38291033277679,19.6537456100734,1.54529289749871));
#11196=CARTESIAN_POINT('Ctrl Pts',(-1.67659613043342,19.8620789434068,1.0960503183159));
#11197=CARTESIAN_POINT('Ctrl Pts',(-1.97028192809006,20.0704122767401,0.646807739133152));
#11198=CARTESIAN_POINT('Ctrl Pts',(-1.99999999999999,20.2787456100735,0.11090935427082));
#11199=CARTESIAN_POINT('Ctrl Pts',(-2.02971807190993,20.4870789434068,-0.424989030591398));
#11200=CARTESIAN_POINT('Ctrl Pts',(-1.78750548470433,20.6954122767402,-0.903949681684127));
#11201=CARTESIAN_POINT('Ctrl Pts',(-1.5452928974987,20.9037456100735,-1.38291033277683));
#11202=CARTESIAN_POINT('Ctrl Pts',(-1.09605031831595,21.1120789434068,-1.67659613043348));
#11203=CARTESIAN_POINT('Ctrl Pts',(-0.646807739133154,21.3204122767401,
-1.97028192809006));
#11204=CARTESIAN_POINT('Ctrl Pts',(-0.110909354270907,21.5287456100735,
-2.));
#11205=CARTESIAN_POINT('Ctrl Pts',(0.424989030591338,21.7370789434068,-2.02971807190994));
#11206=CARTESIAN_POINT('Ctrl Pts',(0.903949681684066,21.9454122767402,-1.78750548470436));
#11207=CARTESIAN_POINT('Ctrl Pts',(1.38291033277679,22.1537456100734,-1.54529289749877));
#11208=CARTESIAN_POINT('Ctrl Pts',(1.67659613043343,22.3620789434069,-1.09605031831595));
#11209=CARTESIAN_POINT('Ctrl Pts',(1.97028192809003,22.5704122767401,-0.646807739133152));
#11210=CARTESIAN_POINT('Ctrl Pts',(2.,22.7787456100735,-0.110909354270945));
#11211=CARTESIAN_POINT('Ctrl Pts',(2.02971807190997,22.9870789434068,0.42498903059134));
#11212=CARTESIAN_POINT('Ctrl Pts',(1.78750548470433,23.1954122767402,0.903949681684009));
#11213=CARTESIAN_POINT('Ctrl Pts',(1.54529289749872,23.4037456100734,1.38291033277679));
#11214=CARTESIAN_POINT('Ctrl Pts',(1.09605031831593,23.6120789434068,1.6765961304334));
#11215=CARTESIAN_POINT('Ctrl Pts',(0.646807739133168,23.8204122767401,1.97028192809006));
#11216=CARTESIAN_POINT('Ctrl Pts',(0.110909354270907,24.0287456100735,1.99999999999992));
#11217=CARTESIAN_POINT('Ctrl Pts',(-0.424989030591338,24.2370789434068,
2.02971807190996));
#11218=CARTESIAN_POINT('Ctrl Pts',(-0.903949681684066,24.4454122767402,
1.78750548470424));
#11219=CARTESIAN_POINT('Ctrl Pts',(-1.38291033277678,24.6537456100735,1.54529289749864));
#11220=CARTESIAN_POINT('Ctrl Pts',(-1.67659613043341,24.8620789434068,1.09605031831588));
#11221=CARTESIAN_POINT('Ctrl Pts',(-1.97028192809005,25.0704122767401,0.646807739133166));
#11222=CARTESIAN_POINT('Ctrl Pts',(-2.,25.2787456100735,0.110909354270855));
#11223=CARTESIAN_POINT('Ctrl Pts',(-2.02971807190995,25.4870789434068,-0.424989030591369));
#11224=CARTESIAN_POINT('Ctrl Pts',(-1.78750548470433,25.6954122767401,-0.903949681684079));
#11225=CARTESIAN_POINT('Ctrl Pts',(-1.54529289749871,25.9037456100735,-1.3829103327768));
#11226=CARTESIAN_POINT('Ctrl Pts',(-1.09605031831593,26.1120789434068,-1.67659613043345));
#11227=CARTESIAN_POINT('Ctrl Pts',(-0.646807739133152,26.3204122767401,
-1.97028192809011));
#11228=CARTESIAN_POINT('Ctrl Pts',(-0.110909354270907,26.5287456100735,
-2.00000000000004));
#11229=CARTESIAN_POINT('Ctrl Pts',(0.424989030591353,26.7370789434068,-2.02971807190995));
#11230=CARTESIAN_POINT('Ctrl Pts',(0.90394968168408,26.9454122767402,-1.78750548470438));
#11231=CARTESIAN_POINT('Ctrl Pts',(1.38291033277679,27.1537456100734,-1.54529289749872));
#11232=CARTESIAN_POINT('Ctrl Pts',(1.6765961304334,27.3620789434068,-1.09605031831597));
#11233=CARTESIAN_POINT('Ctrl Pts',(1.97028192809005,27.5704122767401,-0.64680773913318));
#11234=CARTESIAN_POINT('Ctrl Pts',(1.99999999999997,27.7787456100735,-0.110909354270911));
#11235=CARTESIAN_POINT('Ctrl Pts',(2.02971807190995,27.9870789434068,0.424989030591333));
#11236=CARTESIAN_POINT('Ctrl Pts',(1.78750548470433,28.1954122767402,0.903949681684037));
#11237=CARTESIAN_POINT('Ctrl Pts',(1.5452928974987,28.4037456100735,1.38291033277679));
#11238=CARTESIAN_POINT('Ctrl Pts',(1.09605031831593,28.6120789434068,1.67659613043337));
#11239=CARTESIAN_POINT('Ctrl Pts',(0.646807739133154,28.8204122767401,1.97028192809002));
#11240=CARTESIAN_POINT('Ctrl Pts',(0.110909354270921,29.0287456100735,1.99999999999997));
#11241=CARTESIAN_POINT('Ctrl Pts',(-0.424989030591338,29.2370789434068,
2.02971807190995));
#11242=CARTESIAN_POINT('Ctrl Pts',(-0.903949681684064,29.4454122767402,
1.78750548470427));
#11243=CARTESIAN_POINT('Ctrl Pts',(-1.38291033277679,29.6537456100735,1.54529289749868));
#11244=CARTESIAN_POINT('Ctrl Pts',(-1.67659613043342,29.8620789434068,1.09605031831586));
#11245=CARTESIAN_POINT('Ctrl Pts',(-1.97028192809005,30.0704122767401,0.646807739133123));
#11246=CARTESIAN_POINT('Ctrl Pts',(-2.,30.2787456100735,0.110909354270834));
#11247=CARTESIAN_POINT('Ctrl Pts',(-2.02971807190995,30.4870789434068,-0.424989030591398));
#11248=CARTESIAN_POINT('Ctrl Pts',(-1.78750548470432,30.6954122767402,-0.903949681684113));
#11249=CARTESIAN_POINT('Ctrl Pts',(-1.54529289749872,30.9037456100735,-1.38291033277676));
#11250=CARTESIAN_POINT('Ctrl Pts',(-1.09605031831593,31.1120789434068,-1.67659613043348));
#11251=CARTESIAN_POINT('Ctrl Pts',(-0.646807739133152,31.3204122767401,
-1.97028192809006));
#11252=CARTESIAN_POINT('Ctrl Pts',(-0.110909354270905,31.5287456100735,
-2.));
#11253=CARTESIAN_POINT('Ctrl Pts',(0.42498903059134,31.7370789434068,-2.02971807190996));
#11254=CARTESIAN_POINT('Ctrl Pts',(0.903949681684054,31.9454122767402,-1.78750548470435));
#11255=CARTESIAN_POINT('Ctrl Pts',(1.38291033277679,32.1537456100735,-1.54529289749877));
#11256=CARTESIAN_POINT('Ctrl Pts',(1.67659613043342,32.3620789434069,-1.09605031831598));
#11257=CARTESIAN_POINT('Ctrl Pts',(1.97028192809005,32.5704122767401,-0.646807739133152));
#11258=CARTESIAN_POINT('Ctrl Pts',(2.,32.7787456100735,-0.110909354270917));
#11259=CARTESIAN_POINT('Ctrl Pts',(2.02971807190995,32.9870789434069,0.424989030591311));
#11260=CARTESIAN_POINT('Ctrl Pts',(1.78750548470433,33.1954122767402,0.903949681684009));
#11261=CARTESIAN_POINT('Ctrl Pts',(1.54529289749872,33.4037456100734,1.38291033277681));
#11262=CARTESIAN_POINT('Ctrl Pts',(1.09605031831593,33.6120789434068,1.67659613043341));
#11263=CARTESIAN_POINT('Ctrl Pts',(0.646807739133154,33.8204122767401,1.97028192809006));
#11264=CARTESIAN_POINT('Ctrl Pts',(0.110909354270907,34.0287456100735,1.99999999999993));
#11265=CARTESIAN_POINT('Ctrl Pts',(-0.424989030591338,34.2370789434068,
2.02971807190994));
#11266=CARTESIAN_POINT('Ctrl Pts',(-0.903949681684066,34.4454122767402,
1.78750548470426));
#11267=CARTESIAN_POINT('Ctrl Pts',(-1.38291033277681,34.6537456100735,1.54529289749869));
#11268=CARTESIAN_POINT('Ctrl Pts',(-1.67659613043341,34.8620789434068,1.0960503183159));
#11269=CARTESIAN_POINT('Ctrl Pts',(-1.97028192809005,35.0704122767402,0.646807739133166));
#11270=CARTESIAN_POINT('Ctrl Pts',(-2.,35.2787456100736,0.110909354270855));
#11271=CARTESIAN_POINT('Ctrl Pts',(-2.02971807190995,35.4870789434068,-0.424989030591383));
#11272=CARTESIAN_POINT('Ctrl Pts',(-1.78750548470433,35.6954122767402,-0.903949681684099));
#11273=CARTESIAN_POINT('Ctrl Pts',(-1.54529289749872,35.9037456100735,-1.38291033277681));
#11274=CARTESIAN_POINT('Ctrl Pts',(-1.09605031831593,36.1120789434069,-1.67659613043344));
#11275=CARTESIAN_POINT('Ctrl Pts',(-0.646807739133139,36.3204122767402,
-1.97028192809006));
#11276=CARTESIAN_POINT('Ctrl Pts',(-0.110909354270907,36.5287456100735,
-2.00000000000004));
#11277=CARTESIAN_POINT('Ctrl Pts',(0.424989030591338,36.7370789434068,-2.02971807190996));
#11278=CARTESIAN_POINT('Ctrl Pts',(0.903949681684066,36.9454122767402,-1.78750548470439));
#11279=CARTESIAN_POINT('Ctrl Pts',(1.38291033277679,37.1537456100734,-1.54529289749872));
#11280=CARTESIAN_POINT('Ctrl Pts',(1.67659613043343,37.3620789434069,-1.09605031831598));
#11281=CARTESIAN_POINT('Ctrl Pts',(1.97028192809006,37.5704122767401,-0.646807739133152));
#11282=CARTESIAN_POINT('Ctrl Pts',(2.,37.7787456100735,-0.110909354270952));
#11283=CARTESIAN_POINT('Ctrl Pts',(2.02971807190997,37.9870789434069,0.424989030591333));
#11284=CARTESIAN_POINT('Ctrl Pts',(1.78750548470433,38.1954122767402,0.903949681684023));
#11285=CARTESIAN_POINT('Ctrl Pts',(1.54529289749872,38.4037456100734,1.3829103327768));
#11286=CARTESIAN_POINT('Ctrl Pts',(1.09605031831595,38.6120789434069,1.67659613043338));
#11287=CARTESIAN_POINT('Ctrl Pts',(0.646807739133154,38.8204122767402,1.97028192809006));
#11288=CARTESIAN_POINT('Ctrl Pts',(0.110909354270921,39.0287456100735,1.99999999999997));
#11289=CARTESIAN_POINT('Ctrl Pts',(-0.424989030591324,39.2370789434069,
2.02971807190996));
#11290=CARTESIAN_POINT('Ctrl Pts',(-0.903949681684052,39.4454122767402,
1.78750548470429));
#11291=CARTESIAN_POINT('Ctrl Pts',(-1.38291033277679,39.6537456100735,1.54529289749867));
#11292=CARTESIAN_POINT('Ctrl Pts',(-1.67659613043342,39.8620789434069,1.09605031831587));
#11293=CARTESIAN_POINT('Ctrl Pts',(-1.97028192809005,40.0704122767402,0.646807739133166));
#11294=CARTESIAN_POINT('Ctrl Pts',(-2.,40.2787456100735,0.110909354270834));
#11295=CARTESIAN_POINT('Ctrl Pts',(-2.00308415717522,0.327811454287795,
-0.0144742926159549));
#11296=CARTESIAN_POINT('Ctrl Pts',(-2.02960770809824,0.326083522404792,
-0.0117641501090121));
#11297=CARTESIAN_POINT('Ctrl Pts',(-2.05570512799209,0.320591728514443,
-0.00890360021891084));
#11298=CARTESIAN_POINT('Ctrl Pts',(-2.1162806096187,0.299064621655046,-0.00167442520673255));
#11299=CARTESIAN_POINT('Ctrl Pts',(-2.14909453914282,0.279784636444006,
0.00275906069350319));
#11300=CARTESIAN_POINT('Ctrl Pts',(-2.20027423277635,0.236305190619192,
0.0107637785694441));
#11301=CARTESIAN_POINT('Ctrl Pts',(-2.22004359368015,0.214292607972338,
0.0142777651219529));
#11302=CARTESIAN_POINT('Ctrl Pts',(-2.25554049776359,0.162900143744721,
0.021564697553154));
#11303=CARTESIAN_POINT('Ctrl Pts',(-2.27037406610162,0.133105928183891,
0.0253044485090571));
#11304=CARTESIAN_POINT('Ctrl Pts',(-2.28333129245606,0.0945494429191525,
0.029529898402844));
#11305=CARTESIAN_POINT('Ctrl Pts',(-2.28551379053089,0.087294323511717,
0.0303213415012689));
#11306=CARTESIAN_POINT('Ctrl Pts',(-2.28747252867205,0.0799568405573766,
0.0310811961015807));
#11307=CARTESIAN_POINT('Ctrl Pts',(-2.00000135271328,-0.264728740315192,
0.141133603659935));
#11308=CARTESIAN_POINT('Ctrl Pts',(-1.93317947679614,-0.140205665678286,
0.374694616019038));
#11309=CARTESIAN_POINT('Ctrl Pts',(-1.89576261275035,-0.0714195242393531,
0.563391879075593));
#11310=CARTESIAN_POINT('Ctrl Pts',(-1.85828016234107,-0.0141476745355931,
0.845995304749381));
#11311=CARTESIAN_POINT('Ctrl Pts',(-1.85721582540971,-0.0237125088868792,
0.935184056400945));
#11312=CARTESIAN_POINT('Ctrl Pts',(-1.86061638209651,-0.0666740172427863,
1.06187361715673));
#11313=CARTESIAN_POINT('Ctrl Pts',(-1.86640738686477,-0.101672715288381,
1.11012925637074));
#11314=CARTESIAN_POINT('Ctrl Pts',(-1.88833554246329,-0.235746153313808,
1.21545234876845));
#11315=CARTESIAN_POINT('Ctrl Pts',(-1.9033753276643,-0.335251316849042,
1.26604967753693));
#11316=CARTESIAN_POINT('Ctrl Pts',(-1.9189176957612,-0.518726439558199,
1.34035163842065));
#11317=CARTESIAN_POINT('Ctrl Pts',(-1.92137116451861,-0.585485291115871,
1.36832017615168));
#11318=CARTESIAN_POINT('Ctrl Pts',(-1.93896943688162,-0.724455435049461,
1.40322870297494));
#11319=CARTESIAN_POINT('Ctrl Pts',(-1.95325668725115,-0.796545227124419,
1.40888781048668));
#11320=CARTESIAN_POINT('Ctrl Pts',(-1.99209925627655,-1.01599260874888,
1.41219882843878));
#11321=CARTESIAN_POINT('Ctrl Pts',(-2.00898122237353,-1.16761549888469,
1.40420126611032));
#11322=CARTESIAN_POINT('Ctrl Pts',(-2.01271588366055,-1.60175062040053,
1.36576567629003));
#11323=CARTESIAN_POINT('Ctrl Pts',(-1.95046360827934,-1.85129221142242,
1.32547580954877));
#11324=CARTESIAN_POINT('Ctrl Pts',(-1.69792570410908,-2.14007513561928,
1.27973035876422));
#11325=CARTESIAN_POINT('Ctrl Pts',(-1.50788517190343,-2.24578075342313,
1.26508664601861));
#11326=CARTESIAN_POINT('Ctrl Pts',(-1.03351721040672,-2.37409803162741,
1.24662061906772));
#11327=CARTESIAN_POINT('Ctrl Pts',(-0.753928362614793,-2.39679255199907,
1.24243205928811));
#11328=CARTESIAN_POINT('Ctrl Pts',(-0.218845999430284,-2.35785399723118,
1.24055602083421));
#11329=CARTESIAN_POINT('Ctrl Pts',(0.0368662467341799,-2.29519092886669,
1.24322556456469));
#11330=CARTESIAN_POINT('Ctrl Pts',(0.411239882065782,-2.11406967659605,
1.2495991139221));
#11331=CARTESIAN_POINT('Ctrl Pts',(0.518384719875618,-2.00298884738698,
1.25072899682664));
#11332=CARTESIAN_POINT('Ctrl Pts',(0.571801954928687,-1.83523605217566,
1.25334679757698));
#11333=CARTESIAN_POINT('Ctrl Pts',(0.569023344394799,-1.74044478899434,
1.25599881503435));
#11334=CARTESIAN_POINT('Ctrl Pts',(0.494126240428662,-1.50788563057796,
1.25886663470126));
#11335=CARTESIAN_POINT('Ctrl Pts',(0.421606239831573,-1.37485017740085,
1.26041038383949));
#11336=CARTESIAN_POINT('Ctrl Pts',(0.127609128452456,-0.989034614321357,
1.26907008807672));
#11337=CARTESIAN_POINT('Ctrl Pts',(-0.170570542490676,-0.751894328558357,
1.28023791867232));
#11338=CARTESIAN_POINT('Ctrl Pts',(-0.569600762546571,-0.586703644418381,
1.30640573381989));
#11339=CARTESIAN_POINT('Ctrl Pts',(-0.692371618949951,-0.563856396440986,
1.31685387723007));
#11340=CARTESIAN_POINT('Ctrl Pts',(-0.882581236630141,-0.577499841895708,
1.33968897633028));
#11341=CARTESIAN_POINT('Ctrl Pts',(-0.949730803773584,-0.6053755874494,
1.35084566027416));
#11342=CARTESIAN_POINT('Ctrl Pts',(-1.08267031338154,-0.742643707380371,
1.38530535019886));
#11343=CARTESIAN_POINT('Ctrl Pts',(-1.14980571385887,-0.863823663666268,
1.41045379245241));
#11344=CARTESIAN_POINT('Ctrl Pts',(-1.22863752459304,-1.27359538565792,
1.48274964800499));
#11345=CARTESIAN_POINT('Ctrl Pts',(-1.23841278692706,-1.55826711159036,
1.52914339518866));
#11346=CARTESIAN_POINT('Ctrl Pts',(-1.19858468901873,-1.92998306793573,
1.58589472341859));
#11347=CARTESIAN_POINT('Ctrl Pts',(-1.41479641657991,-0.327027665826027,
0.0242831581950105));
#11348=CARTESIAN_POINT('Ctrl Pts',(-1.34348892337276,-0.181250738802885,
0.26897733822669));
#11349=CARTESIAN_POINT('Ctrl Pts',(-1.3008280875213,-0.0880638424496696,
0.476392819418064));
#11350=CARTESIAN_POINT('Ctrl Pts',(-1.25754057161045,0.0123013660558204,
0.831666797361881));
#11351=CARTESIAN_POINT('Ctrl Pts',(-1.25687388480527,0.0194522591100595,
0.979479411006855));
#11352=CARTESIAN_POINT('Ctrl Pts',(-1.2830830371466,-0.0336379080354797,
1.23391882276437));
#11353=CARTESIAN_POINT('Ctrl Pts',(-1.30959041125068,-0.0938600720654208,
1.34021747917579));
#11354=CARTESIAN_POINT('Ctrl Pts',(-1.38041341547889,-0.261824969553754,
1.53853407301497));
#11355=CARTESIAN_POINT('Ctrl Pts',(-1.42362766577653,-0.369411940643664,
1.63197959161429));
#11356=CARTESIAN_POINT('Ctrl Pts',(-1.51482462448403,-0.553055900414141,
1.7840154902546));
#11357=CARTESIAN_POINT('Ctrl Pts',(-1.55452145207106,-0.616871235334267,
1.84288502733572));
#11358=CARTESIAN_POINT('Ctrl Pts',(-1.61769237293684,-0.76088554847919,
1.90941994885935));
#11359=CARTESIAN_POINT('Ctrl Pts',(-1.63741652204799,-0.839819060706829,
1.91721278463516));
#11360=CARTESIAN_POINT('Ctrl Pts',(-1.67857813189676,-1.07311708366726,
1.92065626175757));
#11361=CARTESIAN_POINT('Ctrl Pts',(-1.69450638574114,-1.22468485755413,
1.91207917479615));
#11362=CARTESIAN_POINT('Ctrl Pts',(-1.69776273723848,-1.63025676912522,
1.87601769283407));
#11363=CARTESIAN_POINT('Ctrl Pts',(-1.63558587031057,-1.8094473554909,1.8484014728917));
#11364=CARTESIAN_POINT('Ctrl Pts',(-1.51744170723058,-1.93391724344097,
1.82161070104937));
#11365=CARTESIAN_POINT('Ctrl Pts',(-1.38720614355509,-2.01215777720118,
1.80651658245784));
#11366=CARTESIAN_POINT('Ctrl Pts',(-0.999318445532683,-2.1000372109959,
1.78142022672165));
#11367=CARTESIAN_POINT('Ctrl Pts',(-0.75320228279494,-2.109345485096,1.77049841986191));
#11368=CARTESIAN_POINT('Ctrl Pts',(-0.291144343481196,-2.05182844476988,
1.75300283223748));
#11369=CARTESIAN_POINT('Ctrl Pts',(-0.0746276920240247,-1.98390441220646,
1.74716065612451));
#11370=CARTESIAN_POINT('Ctrl Pts',(0.192072445804306,-1.83915272276575,
1.73915712563726));
#11371=CARTESIAN_POINT('Ctrl Pts',(0.210347585325089,-1.77773490581458,
1.73080489996179));
#11372=CARTESIAN_POINT('Ctrl Pts',(0.198976982175155,-1.81462152515841,
1.73113541660097));
#11373=CARTESIAN_POINT('Ctrl Pts',(0.213011996067426,-1.79205629656322,
1.73877515384333));
#11374=CARTESIAN_POINT('Ctrl Pts',(0.177186567758258,-1.65070903664641,
1.7504269870299));
#11375=CARTESIAN_POINT('Ctrl Pts',(0.129908624188708,-1.54404411523484,
1.75773877200305));
#11376=CARTESIAN_POINT('Ctrl Pts',(-0.0876107518951426,-1.21505608778235,
1.78559033317587));
#11377=CARTESIAN_POINT('Ctrl Pts',(-0.337497876869364,-0.989695956702306,
1.81129298511067));
#11378=CARTESIAN_POINT('Ctrl Pts',(-0.619417429815987,-0.851281642971048,
1.84410939565886));
#11379=CARTESIAN_POINT('Ctrl Pts',(-0.691821618472955,-0.839216119419207,
1.85456575460658));
#11380=CARTESIAN_POINT('Ctrl Pts',(-0.742506322151624,-0.836948971076064,
1.86696729841403));
#11381=CARTESIAN_POINT('Ctrl Pts',(-0.720038690828119,-0.826234748910869,
1.86596691745099));
#11382=CARTESIAN_POINT('Ctrl Pts',(-0.741001371120147,-0.843622783703197,
1.87515508429125));
#11383=CARTESIAN_POINT('Ctrl Pts',(-0.787635764756597,-0.899635885793011,
1.88970955146323));
#11384=CARTESIAN_POINT('Ctrl Pts',(-0.852118294742336,-1.21903207139812,
1.94900258458685));
#11385=CARTESIAN_POINT('Ctrl Pts',(-0.865431353370241,-1.47313529513962,
1.99195746223939));
#11386=CARTESIAN_POINT('Ctrl Pts',(-0.829509728173782,-1.82164035961998,
2.04637874141716));
#11387=CARTESIAN_POINT('Ctrl Pts',(-1.41479632875941,0.202424372508809,
-0.25799425695406));
#11388=CARTESIAN_POINT('Ctrl Pts',(-1.34782702531429,0.367995784832215,
0.0238273770113642));
#11389=CARTESIAN_POINT('Ctrl Pts',(-1.30808717043028,0.48478124421137,0.280929685456974));
#11390=CARTESIAN_POINT('Ctrl Pts',(-1.27980253042162,0.615948260124595,
0.792619532033457));
#11391=CARTESIAN_POINT('Ctrl Pts',(-1.29321476237305,0.626404567290167,
1.05659684088554));
#11392=CARTESIAN_POINT('Ctrl Pts',(-1.38946357811,0.488938846353634,1.53600410055517));
#11393=CARTESIAN_POINT('Ctrl Pts',(-1.46927966447622,0.34423952699714,1.72959611556546));
#11394=CARTESIAN_POINT('Ctrl Pts',(-1.64804633832672,0.0351654638783543,
1.99593663738672));
#11395=CARTESIAN_POINT('Ctrl Pts',(-1.74809047347069,-0.128192913728382,
2.08305283586927));
#11396=CARTESIAN_POINT('Ctrl Pts',(-1.93188952347472,-0.373532157725284,
2.17842710957436));
#11397=CARTESIAN_POINT('Ctrl Pts',(-2.00679552031709,-0.454457191434216,
2.20361434518665));
#11398=CARTESIAN_POINT('Ctrl Pts',(-2.10891108326887,-0.632484078259461,
2.2307813240385));
#11399=CARTESIAN_POINT('Ctrl Pts',(-2.13408587854556,-0.728563548890991,
2.23545023463704));
#11400=CARTESIAN_POINT('Ctrl Pts',(-2.18470343784499,-1.01580120595979,
2.23985105426332));
#11401=CARTESIAN_POINT('Ctrl Pts',(-2.20504953495422,-1.20449005728727,
2.22965055680831));
#11402=CARTESIAN_POINT('Ctrl Pts',(-2.20926209776938,-1.74080899784122,
2.18228791128134));
#11403=CARTESIAN_POINT('Ctrl Pts',(-2.13571406139752,-2.05748394873335,
2.12938063388729));
#11404=CARTESIAN_POINT('Ctrl Pts',(-1.80914039490605,-2.4116424454986,2.07707686166329));
#11405=CARTESIAN_POINT('Ctrl Pts',(-1.58558544675306,-2.52101501223511,
2.06437413078064));
#11406=CARTESIAN_POINT('Ctrl Pts',(-1.06274917012361,-2.63535508293751,
2.05380211046861));
#11407=CARTESIAN_POINT('Ctrl Pts',(-0.765526424774163,-2.63982623851908,
2.05574575179177));
#11408=CARTESIAN_POINT('Ctrl Pts',(-0.201198256641021,-2.55922793898205,
2.06506565863797));
#11409=CARTESIAN_POINT('Ctrl Pts',(0.0660448366282887,-2.47511972447648,
2.07245950804548));
#11410=CARTESIAN_POINT('Ctrl Pts',(0.475148760175511,-2.24745677674094,
2.08564829134537));
#11411=CARTESIAN_POINT('Ctrl Pts',(0.608134614732898,-2.10455710556735,
2.09040062351607));
#11412=CARTESIAN_POINT('Ctrl Pts',(0.692807377742016,-1.84294516771091,
2.09414100985965));
#11413=CARTESIAN_POINT('Ctrl Pts',(0.695288539321058,-1.71667259554446,
2.09510414856687));
#11414=CARTESIAN_POINT('Ctrl Pts',(0.624899286559479,-1.43522068083482,
2.09446462416269));
#11415=CARTESIAN_POINT('Ctrl Pts',(0.555414215357652,-1.2826933626758,2.0935057350151));
#11416=CARTESIAN_POINT('Ctrl Pts',(0.273957080557801,-0.835699802377016,
2.09178023085904));
#11417=CARTESIAN_POINT('Ctrl Pts',(-0.0144466890476935,-0.553079604701429,
2.09136454656141));
#11418=CARTESIAN_POINT('Ctrl Pts',(-0.45094860176887,-0.336574440271572,
2.10878602648762));
#11419=CARTESIAN_POINT('Ctrl Pts',(-0.595413630263608,-0.298852315146673,
2.11776209928019));
#11420=CARTESIAN_POINT('Ctrl Pts',(-0.85098489192329,-0.305627887932605,
2.14353553496541));
#11421=CARTESIAN_POINT('Ctrl Pts',(-0.96192160586922,-0.346842648185032,
2.15984784684465));
#11422=CARTESIAN_POINT('Ctrl Pts',(-1.15250413694999,-0.533505951798014,
2.20558401172234));
#11423=CARTESIAN_POINT('Ctrl Pts',(-1.23266332711506,-0.683289971881234,
2.23568288668276));
#11424=CARTESIAN_POINT('Ctrl Pts',(-1.32515666438693,-1.13327359192835,
2.31428720538256));
#11425=CARTESIAN_POINT('Ctrl Pts',(-1.33679811649895,-1.43203332580916,
2.36251628262105));
#11426=CARTESIAN_POINT('Ctrl Pts',(-1.29844891076763,-1.81475034924797,
2.42060937990806));
#11427=CARTESIAN_POINT('Ctrl Pts',(-2.00000126489276,0.264723298019645,
-0.141143811489164));
#11428=CARTESIAN_POINT('Ctrl Pts',(-1.93751757873767,0.409040857956806,
0.129544654803658));
#11429=CARTESIAN_POINT('Ctrl Pts',(-1.90302169565935,0.501425562421714,
0.367928745114527));
#11430=CARTESIAN_POINT('Ctrl Pts',(-1.88054212115223,0.589499219533149,
0.806948039420934));
#11431=CARTESIAN_POINT('Ctrl Pts',(-1.89355670297749,0.583239799293228,
1.01230148627963));
#11432=CARTESIAN_POINT('Ctrl Pts',(-1.96699692305992,0.455902737146338,
1.36395889494755));
#11433=CARTESIAN_POINT('Ctrl Pts',(-2.02609664009031,0.336426883774145,
1.4995078927604));
#11434=CARTESIAN_POINT('Ctrl Pts',(-2.15596846531113,0.0612442801182847,
1.67285491314019));
#11435=CARTESIAN_POINT('Ctrl Pts',(-2.22783813535845,-0.0940322899337931,
1.71712292179187));
#11436=CARTESIAN_POINT('Ctrl Pts',(-2.33598259475191,-0.33920269686933,
1.73476325774032));
#11437=CARTESIAN_POINT('Ctrl Pts',(-2.37364523276466,-0.423071247215849,
1.72904949400271));
#11438=CARTESIAN_POINT('Ctrl Pts',(-2.43018814721365,-0.596053964829743,
1.72459007815411));
#11439=CARTESIAN_POINT('Ctrl Pts',(-2.44992604374876,-0.685289715308575,
1.72712526048845));
#11440=CARTESIAN_POINT('Ctrl Pts',(-2.49822456222477,-0.958676731041413,
1.73139362094456));
#11441=CARTESIAN_POINT('Ctrl Pts',(-2.51952437158661,-1.14742069861778,
1.72177264812241));
#11442=CARTESIAN_POINT('Ctrl Pts',(-2.52421524419146,-1.71230284911647,
1.67203589473725));
#11443=CARTESIAN_POINT('Ctrl Pts',(-2.45059179936626,-2.09932880466486,
1.60645497054434));
#11444=CARTESIAN_POINT('Ctrl Pts',(-1.98962439178456,-2.61780033767695,
1.53519651937827));
#11445=CARTESIAN_POINT('Ctrl Pts',(-1.70626447510137,-2.75463798845714,
1.52294419434135));
#11446=CARTESIAN_POINT('Ctrl Pts',(-1.09694793499771,-2.90941590356896,
1.5190025028147));
#11447=CARTESIAN_POINT('Ctrl Pts',(-0.766252504594009,-2.92727330542218,
1.52767939121794));
#11448=CARTESIAN_POINT('Ctrl Pts',(-0.128899912590116,-2.86525349144335,
1.55261884723468));
#11449=CARTESIAN_POINT('Ctrl Pts',(0.177538775386479,-2.78640624113666,
1.56852441648561));
#11450=CARTESIAN_POINT('Ctrl Pts',(0.694316196436971,-2.52237373057128,
1.59609027963019));
#11451=CARTESIAN_POINT('Ctrl Pts',(0.916171749283459,-2.32981104713974,
1.610324720381));
#11452=CARTESIAN_POINT('Ctrl Pts',(1.06563235049552,-1.86355969472816,1.61635239083565));
#11453=CARTESIAN_POINT('Ctrl Pts',(1.05129988764842,-1.66506108797555,1.61232780975798));
#11454=CARTESIAN_POINT('Ctrl Pts',(0.941838959229918,-1.29239727476634,
1.60290427183405));
#11455=CARTESIAN_POINT('Ctrl Pts',(0.847111831000521,-1.11349942484178,
1.59617734685152));
#11456=CARTESIAN_POINT('Ctrl Pts',(0.48917696090542,-0.609678328916015,
1.57525998575984));
#11457=CARTESIAN_POINT('Ctrl Pts',(0.152480645331013,-0.315277976557456,
1.560309480123));
#11458=CARTESIAN_POINT('Ctrl Pts',(-0.401131934499451,-0.0719964417188537,
1.57108236464872));
#11459=CARTESIAN_POINT('Ctrl Pts',(-0.595963630740598,-0.0234925921684045,
1.58005022190368));
#11460=CARTESIAN_POINT('Ctrl Pts',(-0.99105980640179,-0.0461787587522702,
1.61625721288154));
#11461=CARTESIAN_POINT('Ctrl Pts',(-1.19161371881466,-0.12598348672354,
1.64472658966789));
#11462=CARTESIAN_POINT('Ctrl Pts',(-1.49417307921139,-0.432526875475132,
1.71573427762991));
#11463=CARTESIAN_POINT('Ctrl Pts',(-1.5948332762173,-0.647477749754412,
1.75642712767188));
#11464=CARTESIAN_POINT('Ctrl Pts',(-1.70167589423767,-1.18783690618816,
1.84803426880073));
#11465=CARTESIAN_POINT('Ctrl Pts',(-1.70977955005583,-1.51716514225989,
1.89970221556995));
#11466=CARTESIAN_POINT('Ctrl Pts',(-1.66752387161256,-1.92309305756368,
1.96012536190953));
#11467=CARTESIAN_POINT('Ctrl Pts',(-2.58520620102617,0.327022223530482,
-0.0242933660241372));
#11468=CARTESIAN_POINT('Ctrl Pts',(-2.52720813216107,0.450085931081367,
0.235261932595972));
#11469=CARTESIAN_POINT('Ctrl Pts',(-2.49795622088845,0.518069880632045,
0.454927804771985));
#11470=CARTESIAN_POINT('Ctrl Pts',(-2.48128171188284,0.563050178941749,
0.821276546808376));
#11471=CARTESIAN_POINT('Ctrl Pts',(-2.49389864358197,0.540075031296315,
0.968006131673827));
#11472=CARTESIAN_POINT('Ctrl Pts',(-2.54453026800985,0.422866627938986,
1.19191368933997));
#11473=CARTESIAN_POINT('Ctrl Pts',(-2.58291361570442,0.32861424055116,1.26941966995528));
#11474=CARTESIAN_POINT('Ctrl Pts',(-2.66389059229556,0.0873230963582133,
1.34977318889387));
#11475=CARTESIAN_POINT('Ctrl Pts',(-2.70758579724625,-0.0598716661391885,
1.35119300771448));
#11476=CARTESIAN_POINT('Ctrl Pts',(-2.74007566602911,-0.304873236013411,
1.29109940590619));
#11477=CARTESIAN_POINT('Ctrl Pts',(-2.74049494521224,-0.391685302997432,
1.25448464281861));
#11478=CARTESIAN_POINT('Ctrl Pts',(-2.75146521115844,-0.559623851400008,
1.21839883226965));
#11479=CARTESIAN_POINT('Ctrl Pts',(-2.76576620895198,-0.642015881726228,
1.21880028633987));
#11480=CARTESIAN_POINT('Ctrl Pts',(-2.81174568660457,-0.901552256123071,
1.22293618762564));
#11481=CARTESIAN_POINT('Ctrl Pts',(-2.83399920821904,-1.09035133994834,
1.21389473943648));
#11482=CARTESIAN_POINT('Ctrl Pts',(-2.83916839061358,-1.68379670039174,
1.16178387819315));
#11483=CARTESIAN_POINT('Ctrl Pts',(-2.76546953733502,-2.14117366059643,
1.08352930720148));
#11484=CARTESIAN_POINT('Ctrl Pts',(-2.17010838866312,-2.82395822985523,
0.99331617709322));
#11485=CARTESIAN_POINT('Ctrl Pts',(-1.8269435034497,-2.98826096467916,0.981514257902072));
#11486=CARTESIAN_POINT('Ctrl Pts',(-1.13114669987181,-3.18347672420042,
0.984202895160761));
#11487=CARTESIAN_POINT('Ctrl Pts',(-0.766978584413879,-3.21472037232524,
0.99961303064418));
#11488=CARTESIAN_POINT('Ctrl Pts',(-0.0566015685392616,-3.1712790439046,
1.04017203583152));
#11489=CARTESIAN_POINT('Ctrl Pts',(0.289032714144647,-3.09769275779683,
1.0645893249258));
#11490=CARTESIAN_POINT('Ctrl Pts',(0.913483632698393,-2.79729068440162,
1.10653226791493));
#11491=CARTESIAN_POINT('Ctrl Pts',(1.22420888383399,-2.55506498871208,1.13024881724595));
#11492=CARTESIAN_POINT('Ctrl Pts',(1.43845732324901,-1.88417422174541,1.13856377181168));
#11493=CARTESIAN_POINT('Ctrl Pts',(1.40731123597572,-1.61344958040663,1.12955147094911));
#11494=CARTESIAN_POINT('Ctrl Pts',(1.25877863190032,-1.14957386869789,1.11134391950535));
#11495=CARTESIAN_POINT('Ctrl Pts',(1.13880944664334,-0.944305487007855,
1.09884895868796));
#11496=CARTESIAN_POINT('Ctrl Pts',(0.704396841252997,-0.383656855455022,
1.05873974066059));
#11497=CARTESIAN_POINT('Ctrl Pts',(0.3194079797097,-0.0774763484135167,
1.02925441368461));
#11498=CARTESIAN_POINT('Ctrl Pts',(-0.351315267230051,0.19258155683384,
1.03337870280986));
#11499=CARTESIAN_POINT('Ctrl Pts',(-0.596513631217612,0.251867130809852,
1.0423383445272));
#11500=CARTESIAN_POINT('Ctrl Pts',(-1.13113472088033,0.213270370428087,
1.08897889079772));
#11501=CARTESIAN_POINT('Ctrl Pts',(-1.42130583176012,0.0948756747378918,
1.12960533249102));
#11502=CARTESIAN_POINT('Ctrl Pts',(-1.83584202147282,-0.331547799152291,
1.22588454353743));
#11503=CARTESIAN_POINT('Ctrl Pts',(-1.95700322531958,-0.611665527627663,
1.277171368661));
#11504=CARTESIAN_POINT('Ctrl Pts',(-2.07819512408842,-1.242400220448,1.38178133221873));
#11505=CARTESIAN_POINT('Ctrl Pts',(-2.08276098361269,-1.6022969587106,1.43688814851895));
#11506=CARTESIAN_POINT('Ctrl Pts',(-2.03659883245755,-2.03143576587941,
1.49964134391094));
#11507=CARTESIAN_POINT('Ctrl Pts',(-2.58520628884668,-0.202429814804338,
0.257984049124923));
#11508=CARTESIAN_POINT('Ctrl Pts',(-2.52287003021952,-0.0991605925537074,
0.48041189381135));
#11509=CARTESIAN_POINT('Ctrl Pts',(-2.49069713797941,-0.0547752060290418,
0.650390938733111));
#11510=CARTESIAN_POINT('Ctrl Pts',(-2.45901975307171,-0.0405967151270361,
0.860323812136826));
#11511=CARTESIAN_POINT('Ctrl Pts',(-2.45755776601418,-0.0668772768837554,
0.890888701795052));
#11512=CARTESIAN_POINT('Ctrl Pts',(-2.43814972704647,-0.0997101264501223,
0.889828411549012));
#11513=CARTESIAN_POINT('Ctrl Pts',(-2.42322436247891,-0.109485358511338,
0.880041033565627));
#11514=CARTESIAN_POINT('Ctrl Pts',(-2.39625766944769,-0.209667337073921,
0.892370624522099));
#11515=CARTESIAN_POINT('Ctrl Pts',(-2.38312298955208,-0.301090693054413,
0.900119763459602));
#11516=CARTESIAN_POINT('Ctrl Pts',(-2.32301076703839,-0.484396978702216,
0.896687786586603));
#11517=CARTESIAN_POINT('Ctrl Pts',(-2.2882208769662,-0.554099346897494,
0.893755324967696));
#11518=CARTESIAN_POINT('Ctrl Pts',(-2.26024650082642,-0.688025321619785,
0.897037457090494));
#11519=CARTESIAN_POINT('Ctrl Pts',(-2.26909685245436,-0.753271393542086,
0.90056283633815));
#11520=CARTESIAN_POINT('Ctrl Pts',(-2.30562038065636,-0.958868133830514,
0.903741395119929));
#11521=CARTESIAN_POINT('Ctrl Pts',(-2.32345605900597,-1.11054614021518,
0.896323357424417));
#11522=CARTESIAN_POINT('Ctrl Pts',(-2.32766903008263,-1.57324447167574,
0.855513659745901));
#11523=CARTESIAN_POINT('Ctrl Pts',(-2.26534134624811,-1.89313706735396,
0.802550146205944));
#11524=CARTESIAN_POINT('Ctrl Pts',(-1.8784097009876,-2.34623302779759,0.737850016479276));
#11525=CARTESIAN_POINT('Ctrl Pts',(-1.62856420025181,-2.47940372964513,
0.723656709579273));
#11526=CARTESIAN_POINT('Ctrl Pts',(-1.0677159752808,-2.64815885225886,0.711821011413811));
#11527=CARTESIAN_POINT('Ctrl Pts',(-0.754654442434687,-2.68423961890214,
0.7143656987144));
#11528=CARTESIAN_POINT('Ctrl Pts',(-0.146547655379389,-2.66387954969245,
0.728109209430922));
#11529=CARTESIAN_POINT('Ctrl Pts',(0.148360185492318,-2.60647744552693,
0.739290473004851));
#11530=CARTESIAN_POINT('Ctrl Pts',(0.630407318327205,-2.38898663042632,
0.760041102206871));
#11531=CARTESIAN_POINT('Ctrl Pts',(0.826421854426146,-2.22824278895934,
0.770653093691493));
#11532=CARTESIAN_POINT('Ctrl Pts',(0.944626927682175,-1.85585057919288,
0.775558178553095));
#11533=CARTESIAN_POINT('Ctrl Pts',(0.925034692722124,-1.68883328142547,
0.773222476225436));
#11534=CARTESIAN_POINT('Ctrl Pts',(0.811065913099062,-1.36506222450943,
0.767306282372666));
#11535=CARTESIAN_POINT('Ctrl Pts',(0.713303855474414,-1.20565623956688,
0.763081995675995));
#11536=CARTESIAN_POINT('Ctrl Pts',(0.34282900880003,-0.763013140860391,
0.752549842977497));
#11537=CARTESIAN_POINT('Ctrl Pts',(-0.00364320811200702,-0.51409270041443,
0.749182852233819));
#11538=CARTESIAN_POINT('Ctrl Pts',(-0.51978409527715,-0.322125645865647,
0.768702071980997));
#11539=CARTESIAN_POINT('Ctrl Pts',(-0.692921619426966,-0.288496673462745,
0.779141999853542));
#11540=CARTESIAN_POINT('Ctrl Pts',(-1.02265615110868,-0.318050712715351,
0.812410654246396));
#11541=CARTESIAN_POINT('Ctrl Pts',(-1.17942291671907,-0.38451642598792,
0.835724403097336));
#11542=CARTESIAN_POINT('Ctrl Pts',(-1.42433925564296,-0.641664631057489,
0.895455616106331));
#11543=CARTESIAN_POINT('Ctrl Pts',(-1.51197566296117,-0.828011441539482,
0.931198033441523));
#11544=CARTESIAN_POINT('Ctrl Pts',(-1.60515675444377,-1.32815869991775,
1.016496711423));
#11545=CARTESIAN_POINT('Ctrl Pts',(-1.61139422048387,-1.6433989280412,1.06632932813794));
#11546=CARTESIAN_POINT('Ctrl Pts',(-1.5676596498637,-2.03832577625144,1.12541070542012));
#11547=CARTESIAN_POINT('Ctrl Pts',(-2.00000135271328,-0.264728740315192,
0.141133603659935));
#11548=CARTESIAN_POINT('Ctrl Pts',(-1.93317947679614,-0.140205665678286,
0.374694616019038));
#11549=CARTESIAN_POINT('Ctrl Pts',(-1.89576261275035,-0.0714195242393531,
0.563391879075593));
#11550=CARTESIAN_POINT('Ctrl Pts',(-1.85828016234107,-0.0141476745355931,
0.845995304749381));
#11551=CARTESIAN_POINT('Ctrl Pts',(-1.85721582540971,-0.0237125088868792,
0.935184056400945));
#11552=CARTESIAN_POINT('Ctrl Pts',(-1.86061638209651,-0.0666740172427863,
1.06187361715673));
#11553=CARTESIAN_POINT('Ctrl Pts',(-1.86640738686477,-0.101672715288381,
1.11012925637074));
#11554=CARTESIAN_POINT('Ctrl Pts',(-1.88833554246329,-0.235746153313808,
1.21545234876845));
#11555=CARTESIAN_POINT('Ctrl Pts',(-1.9033753276643,-0.335251316849042,
1.26604967753693));
#11556=CARTESIAN_POINT('Ctrl Pts',(-1.9189176957612,-0.518726439558199,
1.34035163842065));
#11557=CARTESIAN_POINT('Ctrl Pts',(-1.92137116451861,-0.585485291115871,
1.36832017615168));
#11558=CARTESIAN_POINT('Ctrl Pts',(-1.93896943688162,-0.724455435049461,
1.40322870297494));
#11559=CARTESIAN_POINT('Ctrl Pts',(-1.95325668725115,-0.796545227124419,
1.40888781048668));
#11560=CARTESIAN_POINT('Ctrl Pts',(-1.99209925627655,-1.01599260874888,
1.41219882843878));
#11561=CARTESIAN_POINT('Ctrl Pts',(-2.00898122237353,-1.16761549888469,
1.40420126611032));
#11562=CARTESIAN_POINT('Ctrl Pts',(-2.01271588366055,-1.60175062040053,
1.36576567629003));
#11563=CARTESIAN_POINT('Ctrl Pts',(-1.95046360827934,-1.85129221142242,
1.32547580954877));
#11564=CARTESIAN_POINT('Ctrl Pts',(-1.69792570410908,-2.14007513561928,
1.27973035876422));
#11565=CARTESIAN_POINT('Ctrl Pts',(-1.50788517190343,-2.24578075342313,
1.26508664601861));
#11566=CARTESIAN_POINT('Ctrl Pts',(-1.03351721040672,-2.37409803162741,
1.24662061906772));
#11567=CARTESIAN_POINT('Ctrl Pts',(-0.753928362614793,-2.39679255199907,
1.24243205928811));
#11568=CARTESIAN_POINT('Ctrl Pts',(-0.218845999430284,-2.35785399723118,
1.24055602083421));
#11569=CARTESIAN_POINT('Ctrl Pts',(0.0368662467341799,-2.29519092886669,
1.24322556456469));
#11570=CARTESIAN_POINT('Ctrl Pts',(0.411239882065782,-2.11406967659605,
1.2495991139221));
#11571=CARTESIAN_POINT('Ctrl Pts',(0.518384719875618,-2.00298884738698,
1.25072899682664));
#11572=CARTESIAN_POINT('Ctrl Pts',(0.571801954928687,-1.83523605217566,
1.25334679757698));
#11573=CARTESIAN_POINT('Ctrl Pts',(0.569023344394799,-1.74044478899434,
1.25599881503435));
#11574=CARTESIAN_POINT('Ctrl Pts',(0.494126240428662,-1.50788563057796,
1.25886663470126));
#11575=CARTESIAN_POINT('Ctrl Pts',(0.421606239831573,-1.37485017740085,
1.26041038383949));
#11576=CARTESIAN_POINT('Ctrl Pts',(0.127609128452456,-0.989034614321357,
1.26907008807672));
#11577=CARTESIAN_POINT('Ctrl Pts',(-0.170570542490676,-0.751894328558357,
1.28023791867232));
#11578=CARTESIAN_POINT('Ctrl Pts',(-0.569600762546571,-0.586703644418381,
1.30640573381989));
#11579=CARTESIAN_POINT('Ctrl Pts',(-0.692371618949951,-0.563856396440986,
1.31685387723007));
#11580=CARTESIAN_POINT('Ctrl Pts',(-0.882581236630141,-0.577499841895708,
1.33968897633028));
#11581=CARTESIAN_POINT('Ctrl Pts',(-0.949730803773584,-0.6053755874494,
1.35084566027416));
#11582=CARTESIAN_POINT('Ctrl Pts',(-1.08267031338154,-0.742643707380371,
1.38530535019886));
#11583=CARTESIAN_POINT('Ctrl Pts',(-1.14980571385887,-0.863823663666268,
1.41045379245241));
#11584=CARTESIAN_POINT('Ctrl Pts',(-1.22863752459304,-1.27359538565792,
1.48274964800499));
#11585=CARTESIAN_POINT('Ctrl Pts',(-1.23841278692706,-1.55826711159036,
1.52914339518866));
#11586=CARTESIAN_POINT('Ctrl Pts',(-1.19858468901873,-1.92998306793573,
1.58589472341859));
#11587=CARTESIAN_POINT('Origin',(-2.,-2.08166817117217E-14,-3.46944695195361E-14));
#11588=CARTESIAN_POINT('Origin',(-1.43305428031565,-1.92653806274973,1.77301004266414));
#11589=CARTESIAN_POINT('Origin',(-1.43305428031565,-1.92653806274973,1.77301004266414));
#11590=CARTESIAN_POINT('Origin',(-2.,-2.08166817117217E-14,-3.46944695195361E-14));
#11591=CARTESIAN_POINT('Origin',(-1.99999999999999,40.0000000000001,-6.24500451351651E-14));
#11592=CARTESIAN_POINT('Origin',(-1.99999999999999,40.0000000000001,-6.24500451351651E-14));
#11593=CARTESIAN_POINT('Ctrl Pts',(-2.00000000001811,42.8890026416775,-1.69451425055562));
#11594=CARTESIAN_POINT('Ctrl Pts',(-2.00000000001811,42.7138340471106,-1.69451425055564));
#11595=CARTESIAN_POINT('Ctrl Pts',(-2.00000000001811,42.5195868694293,-1.69664685121079));
#11596=CARTESIAN_POINT('Ctrl Pts',(-2.00000000001818,42.1727041659024,-1.69763022720131));
#11597=CARTESIAN_POINT('Ctrl Pts',(-2.00000000001809,42.0075453806213,-1.69643582812033));
#11598=CARTESIAN_POINT('Ctrl Pts',(-2.000000000018,41.5447432182596,-1.67506238348623));
#11599=CARTESIAN_POINT('Ctrl Pts',(-2.00000000001759,41.2824586218001,-1.63529714422004));
#11600=CARTESIAN_POINT('Ctrl Pts',(-2.00000000001559,40.8726877368524,-1.45751662005935));
#11601=CARTESIAN_POINT('Ctrl Pts',(-2.00000000001428,40.7146168625301,-1.32576584773803));
#11602=CARTESIAN_POINT('Ctrl Pts',(-2.00000000000915,40.4347106414413,-0.836444527344903));
#11603=CARTESIAN_POINT('Ctrl Pts',(-2.00000000000487,40.3213171458309,-0.475216515464907));
#11604=CARTESIAN_POINT('Ctrl Pts',(-2.,40.247426591683,0.0357782298078951));
#11605=CARTESIAN_POINT('Ctrl Pts',(-1.50000000001812,42.8890026416775,-1.69451425056007));
#11606=CARTESIAN_POINT('Ctrl Pts',(-1.50000000001811,42.7138340471107,-1.6945142505601));
#11607=CARTESIAN_POINT('Ctrl Pts',(-1.50000000001814,42.5195868694296,-1.69664685121553));
#11608=CARTESIAN_POINT('Ctrl Pts',(-1.50000000001815,42.1727041659021,-1.69763022720547));
#11609=CARTESIAN_POINT('Ctrl Pts',(-1.50000000001812,42.0075453806213,-1.69643582812505));
#11610=CARTESIAN_POINT('Ctrl Pts',(-1.50000000001802,41.5447432182596,-1.6750623834901));
#11611=CARTESIAN_POINT('Ctrl Pts',(-1.50000000001758,41.2824586218004,-1.635297144225));
#11612=CARTESIAN_POINT('Ctrl Pts',(-1.50000000001562,40.8726877368527,-1.45751662006339));
#11613=CARTESIAN_POINT('Ctrl Pts',(-1.50000000001431,40.7146168625313,-1.32576584774273));
#11614=CARTESIAN_POINT('Ctrl Pts',(-1.50000000000914,40.4347106414414,-0.836444527349893));
#11615=CARTESIAN_POINT('Ctrl Pts',(-1.50000000000502,40.321317145827,-0.475216515469928));
#11616=CARTESIAN_POINT('Ctrl Pts',(-1.5,40.2474265916837,0.0357782298028141));
#11617=CARTESIAN_POINT('Ctrl Pts',(-1.50000000002261,42.8890026416775,-2.19451425056016));
#11618=CARTESIAN_POINT('Ctrl Pts',(-1.5000000000226,42.6924352393214,-2.19451425056018));
#11619=CARTESIAN_POINT('Ctrl Pts',(-1.50000000002262,42.5242279803483,-2.196635703513));
#11620=CARTESIAN_POINT('Ctrl Pts',(-1.50000000002264,42.1708979670303,-2.19763735653693));
#11621=CARTESIAN_POINT('Ctrl Pts',(-1.50000000002256,41.9983311272475,-2.19654321697105));
#11622=CARTESIAN_POINT('Ctrl Pts',(-1.50000000002256,41.4939715199041,-2.1732505327887));
#11623=CARTESIAN_POINT('Ctrl Pts',(-1.50000000002207,41.1721096008011,-2.1324514159462));
#11624=CARTESIAN_POINT('Ctrl Pts',(-1.50000000001927,40.5850276451855,-1.87774381002253));
#11625=CARTESIAN_POINT('Ctrl Pts',(-1.50000000001706,40.3267157332556,-1.65463617720806));
#11626=CARTESIAN_POINT('Ctrl Pts',(-1.50000000001012,39.9545934323558,-1.00410633608771));
#11627=CARTESIAN_POINT('Ctrl Pts',(-1.50000000000546,39.831903366932,-0.584389540167537));
#11628=CARTESIAN_POINT('Ctrl Pts',(-1.50000000000002,39.752573408318,-0.0357782298130924));
#11629=CARTESIAN_POINT('Ctrl Pts',(-2.00000000002259,42.8890026416775,-2.19451425055564));
#11630=CARTESIAN_POINT('Ctrl Pts',(-2.0000000000226,42.6924352393214,-2.19451425055565));
#11631=CARTESIAN_POINT('Ctrl Pts',(-2.00000000002263,42.5242279803487,-2.19663570350848));
#11632=CARTESIAN_POINT('Ctrl Pts',(-2.00000000002263,42.17089796703,-2.19763735653241));
#11633=CARTESIAN_POINT('Ctrl Pts',(-2.00000000002255,41.9983311272475,-2.19654321696658));
#11634=CARTESIAN_POINT('Ctrl Pts',(-2.00000000002255,41.4939715199041,-2.17325053278423));
#11635=CARTESIAN_POINT('Ctrl Pts',(-2.00000000002206,41.1721096008009,-2.13245141594075));
#11636=CARTESIAN_POINT('Ctrl Pts',(-2.00000000001923,40.5850276451852,-1.87774381001891));
#11637=CARTESIAN_POINT('Ctrl Pts',(-2.00000000001706,40.3267157332544,-1.65463617720347));
#11638=CARTESIAN_POINT('Ctrl Pts',(-2.00000000001007,39.9545934323557,-1.0041063360826));
#11639=CARTESIAN_POINT('Ctrl Pts',(-2.00000000000546,39.8319033669359,-0.58438954016253));
#11640=CARTESIAN_POINT('Ctrl Pts',(-2.,39.7525734083173,-0.03577822980802));
#11641=CARTESIAN_POINT('Ctrl Pts',(-2.50000000002261,42.8890026416775,-2.19451425055115));
#11642=CARTESIAN_POINT('Ctrl Pts',(-2.5000000000226,42.6924352393213,-2.19451425055115));
#11643=CARTESIAN_POINT('Ctrl Pts',(-2.50000000002264,42.524227980349,-2.19663570350397));
#11644=CARTESIAN_POINT('Ctrl Pts',(-2.50000000002262,42.1708979670296,-2.19763735652791));
#11645=CARTESIAN_POINT('Ctrl Pts',(-2.50000000002255,41.9983311272475,-2.19654321696204));
#11646=CARTESIAN_POINT('Ctrl Pts',(-2.50000000002259,41.493971519904,-2.17325053277969));
#11647=CARTESIAN_POINT('Ctrl Pts',(-2.5000000000221,41.1721096008005,-2.13245141593522));
#11648=CARTESIAN_POINT('Ctrl Pts',(-2.50000000001924,40.5850276451849,-1.87774381001523));
#11649=CARTESIAN_POINT('Ctrl Pts',(-2.50000000001709,40.3267157332532,-1.65463617719887));
#11650=CARTESIAN_POINT('Ctrl Pts',(-2.50000000001009,39.9545934323556,-1.00410633607742));
#11651=CARTESIAN_POINT('Ctrl Pts',(-2.50000000000545,39.8319033669398,-0.584389540157467));
#11652=CARTESIAN_POINT('Ctrl Pts',(-2.50000000000002,39.7525734083165,-0.0357782298028245));
#11653=CARTESIAN_POINT('Ctrl Pts',(-2.50000000001813,42.8890026416775,-1.69451425055113));
#11654=CARTESIAN_POINT('Ctrl Pts',(-2.50000000001811,42.7138340471106,-1.69451425055112));
#11655=CARTESIAN_POINT('Ctrl Pts',(-2.50000000001808,42.519586869429,-1.69664685120596));
#11656=CARTESIAN_POINT('Ctrl Pts',(-2.50000000001821,42.1727041659027,-1.6976302271971));
#11657=CARTESIAN_POINT('Ctrl Pts',(-2.50000000001814,42.0075453806212,-1.69643582811551));
#11658=CARTESIAN_POINT('Ctrl Pts',(-2.50000000001799,41.5447432182596,-1.67506238348225));
#11659=CARTESIAN_POINT('Ctrl Pts',(-2.50000000001761,41.2824586217998,-1.63529714421497));
#11660=CARTESIAN_POINT('Ctrl Pts',(-2.5000000000156,40.872687736852,-1.45751662005523));
#11661=CARTESIAN_POINT('Ctrl Pts',(-2.50000000001424,40.7146168625289,-1.32576584773326));
#11662=CARTESIAN_POINT('Ctrl Pts',(-2.50000000000921,40.4347106414412,-0.836444527339844));
#11663=CARTESIAN_POINT('Ctrl Pts',(-2.50000000000473,40.3213171458348,-0.475216515459863));
#11664=CARTESIAN_POINT('Ctrl Pts',(-2.5,40.2474265916822,0.0357782298130767));
#11665=CARTESIAN_POINT('Ctrl Pts',(-2.00000000001811,42.8890026416775,-1.69451425055562));
#11666=CARTESIAN_POINT('Ctrl Pts',(-2.00000000001811,42.7138340471106,-1.69451425055564));
#11667=CARTESIAN_POINT('Ctrl Pts',(-2.00000000001811,42.5195868694293,-1.69664685121079));
#11668=CARTESIAN_POINT('Ctrl Pts',(-2.00000000001818,42.1727041659024,-1.69763022720131));
#11669=CARTESIAN_POINT('Ctrl Pts',(-2.00000000001809,42.0075453806213,-1.69643582812033));
#11670=CARTESIAN_POINT('Ctrl Pts',(-2.000000000018,41.5447432182596,-1.67506238348623));
#11671=CARTESIAN_POINT('Ctrl Pts',(-2.00000000001759,41.2824586218001,-1.63529714422004));
#11672=CARTESIAN_POINT('Ctrl Pts',(-2.00000000001559,40.8726877368524,-1.45751662005935));
#11673=CARTESIAN_POINT('Ctrl Pts',(-2.00000000001428,40.7146168625301,-1.32576584773803));
#11674=CARTESIAN_POINT('Ctrl Pts',(-2.00000000000915,40.4347106414413,-0.836444527344903));
#11675=CARTESIAN_POINT('Ctrl Pts',(-2.00000000000487,40.3213171458309,-0.475216515464907));
#11676=CARTESIAN_POINT('Ctrl Pts',(-2.,40.247426591683,0.0357782298078951));
#11677=CARTESIAN_POINT('Origin',(-2.0000000000128,41.3499760178345,-1.22177579428992));
#11678=CARTESIAN_POINT('',(0.,0.,0.));
#11679=CARTESIAN_POINT('Origin',(22.9603057217174,0.,-2.33853588412019));
#11680=CARTESIAN_POINT('',(22.9603057217174,1.72563323017097E-31,-4.3385358841202));
#11681=CARTESIAN_POINT('Origin',(22.9603057217174,0.,-2.33853588412019));
#11682=CARTESIAN_POINT('',(22.9603057217174,1.2,-4.3385358841202));
#11683=CARTESIAN_POINT('',(22.9603057217174,1.72563323017097E-31,-4.3385358841202));
#11684=CARTESIAN_POINT('Origin',(22.9603057217174,1.2,-2.33853588412019));
#11685=CARTESIAN_POINT('Ctrl Pts',(-28.2500418808544,1.2,-2.07888836971772));
#11686=CARTESIAN_POINT('Ctrl Pts',(-28.2500418808544,-0.527999999999998,
-2.07888836971772));
#11687=CARTESIAN_POINT('Ctrl Pts',(-27.9613439331009,1.2,-1.81555449964671));
#11688=CARTESIAN_POINT('Ctrl Pts',(-27.9613439331009,-0.527999999999998,
-1.81555449964671));
#11689=CARTESIAN_POINT('Ctrl Pts',(-27.180603234679,1.2,-1.04385836116026));
#11690=CARTESIAN_POINT('Ctrl Pts',(-27.180603234679,-0.527999999999998,
-1.04385836116026));
#11691=CARTESIAN_POINT('Ctrl Pts',(-25.9983030006616,1.2,-0.24124876693352));
#11692=CARTESIAN_POINT('Ctrl Pts',(-25.9983030006616,-0.527999999999998,
-0.24124876693352));
#11693=CARTESIAN_POINT('Ctrl Pts',(-24.2346861695509,1.2,-0.210983790359477));
#11694=CARTESIAN_POINT('Ctrl Pts',(-24.2346861695509,-0.527999999999998,
-0.210983790359477));
#11695=CARTESIAN_POINT('Ctrl Pts',(-23.517870169039,1.2,-1.68305705631707));
#11696=CARTESIAN_POINT('Ctrl Pts',(-23.517870169039,-0.527999999999998,
-1.68305705631707));
#11697=CARTESIAN_POINT('Ctrl Pts',(-23.2233109717715,1.2,-3.05602157557454));
#11698=CARTESIAN_POINT('Ctrl Pts',(-23.2233109717715,-0.527999999999998,
-3.05602157557454));
#11699=CARTESIAN_POINT('Ctrl Pts',(-22.1784263046757,1.2,-3.93337248074442));
#11700=CARTESIAN_POINT('Ctrl Pts',(-22.1784263046757,-0.527999999999998,
-3.93337248074442));
#11701=CARTESIAN_POINT('Ctrl Pts',(-19.19441431546,1.2,-4.74815122044273));
#11702=CARTESIAN_POINT('Ctrl Pts',(-19.19441431546,-0.527999999999998,-4.74815122044273));
#11703=CARTESIAN_POINT('Ctrl Pts',(-15.7509580358841,1.2,-4.44216895895114));
#11704=CARTESIAN_POINT('Ctrl Pts',(-15.7509580358841,-0.527999999999998,
-4.44216895895114));
#11705=CARTESIAN_POINT('Ctrl Pts',(-12.7021174144063,1.2,-4.06331666259747));
#11706=CARTESIAN_POINT('Ctrl Pts',(-12.7021174144063,-0.527999999999998,
-4.06331666259747));
#11707=CARTESIAN_POINT('Ctrl Pts',(-11.3962777017639,1.2,-3.64648316501468));
#11708=CARTESIAN_POINT('Ctrl Pts',(-11.3962777017639,-0.527999999999998,
-3.64648316501468));
#11709=CARTESIAN_POINT('Ctrl Pts',(-11.2344759364774,1.2,-2.80455171594097));
#11710=CARTESIAN_POINT('Ctrl Pts',(-11.2344759364774,-0.527999999999998,
-2.80455171594097));
#11711=CARTESIAN_POINT('Ctrl Pts',(-11.1732737269437,1.2,-1.7662619507528));
#11712=CARTESIAN_POINT('Ctrl Pts',(-11.1732737269437,-0.527999999999998,
-1.7662619507528));
#11713=CARTESIAN_POINT('Ctrl Pts',(-12.7612302838612,1.2,-1.89361059761595));
#11714=CARTESIAN_POINT('Ctrl Pts',(-12.7612302838612,-0.527999999999998,
-1.89361059761595));
#11715=CARTESIAN_POINT('Ctrl Pts',(-13.9972305202523,1.2,-1.67844839769156));
#11716=CARTESIAN_POINT('Ctrl Pts',(-13.9972305202523,-0.527999999999998,
-1.67844839769156));
#11717=CARTESIAN_POINT('Ctrl Pts',(-15.6400181726054,1.2,-2.29491586659866));
#11718=CARTESIAN_POINT('Ctrl Pts',(-15.6400181726054,-0.527999999999998,
-2.29491586659866));
#11719=CARTESIAN_POINT('Ctrl Pts',(-16.7051564115516,1.2,0.0418535888021335));
#11720=CARTESIAN_POINT('Ctrl Pts',(-16.7051564115516,-0.527999999999998,
0.0418535888021335));
#11721=CARTESIAN_POINT('Ctrl Pts',(-13.0664970088623,1.2,0.88071809162054));
#11722=CARTESIAN_POINT('Ctrl Pts',(-13.0664970088623,-0.527999999999998,
0.88071809162054));
#11723=CARTESIAN_POINT('Ctrl Pts',(-10.5984973129989,1.2,0.680667707785562));
#11724=CARTESIAN_POINT('Ctrl Pts',(-10.5984973129989,-0.527999999999998,
0.680667707785562));
#11725=CARTESIAN_POINT('Ctrl Pts',(-7.82942308877726,1.2,0.695565326486597));
#11726=CARTESIAN_POINT('Ctrl Pts',(-7.82942308877726,-0.527999999999998,
0.695565326486597));
#11727=CARTESIAN_POINT('Ctrl Pts',(-6.07620266579566,1.2,2.85997113365485));
#11728=CARTESIAN_POINT('Ctrl Pts',(-6.07620266579566,-0.527999999999998,
2.85997113365485));
#11729=CARTESIAN_POINT('Ctrl Pts',(-3.9066933893458,1.2,4.14091208560258));
#11730=CARTESIAN_POINT('Ctrl Pts',(-3.9066933893458,-0.527999999999998,
4.14091208560258));
#11731=CARTESIAN_POINT('Ctrl Pts',(-2.0279101215411,1.2,5.46819912841997));
#11732=CARTESIAN_POINT('Ctrl Pts',(-2.0279101215411,-0.527999999999998,
5.46819912841997));
#11733=CARTESIAN_POINT('Ctrl Pts',(0.00386116068497311,1.2,5.86471136207473));
#11734=CARTESIAN_POINT('Ctrl Pts',(0.00386116068497311,-0.527999999999998,
5.86471136207473));
#11735=CARTESIAN_POINT('Ctrl Pts',(2.39576994688095,1.2,5.73794061249253));
#11736=CARTESIAN_POINT('Ctrl Pts',(2.39576994688095,-0.527999999999998,
5.73794061249253));
#11737=CARTESIAN_POINT('Ctrl Pts',(5.15590481840992,1.2,5.78580883625202));
#11738=CARTESIAN_POINT('Ctrl Pts',(5.15590481840992,-0.527999999999998,
5.78580883625202));
#11739=CARTESIAN_POINT('Ctrl Pts',(7.73518803149787,1.2,5.79127386586831));
#11740=CARTESIAN_POINT('Ctrl Pts',(7.73518803149787,-0.527999999999998,
5.79127386586831));
#11741=CARTESIAN_POINT('Ctrl Pts',(9.45734572072178,1.2,4.67363967594622));
#11742=CARTESIAN_POINT('Ctrl Pts',(9.45734572072178,-0.527999999999998,
4.67363967594622));
#11743=CARTESIAN_POINT('Ctrl Pts',(9.17706365495184,1.2,2.96306509995752));
#11744=CARTESIAN_POINT('Ctrl Pts',(9.17706365495184,-0.527999999999998,
2.96306509995752));
#11745=CARTESIAN_POINT('Ctrl Pts',(7.81796360098053,1.2,3.18513163158631));
#11746=CARTESIAN_POINT('Ctrl Pts',(7.81796360098053,-0.527999999999998,
3.18513163158631));
#11747=CARTESIAN_POINT('Ctrl Pts',(6.59699346312693,1.2,3.38520430984983));
#11748=CARTESIAN_POINT('Ctrl Pts',(6.59699346312693,-0.527999999999998,
3.38520430984983));
#11749=CARTESIAN_POINT('Ctrl Pts',(5.93021602745299,1.2,1.85802575211607));
#11750=CARTESIAN_POINT('Ctrl Pts',(5.93021602745299,-0.527999999999998,
1.85802575211607));
#11751=CARTESIAN_POINT('Ctrl Pts',(6.62071623580517,1.2,0.188782666588939));
#11752=CARTESIAN_POINT('Ctrl Pts',(6.62071623580517,-0.527999999999998,
0.188782666588939));
#11753=CARTESIAN_POINT('Ctrl Pts',(8.32325294445203,1.2,-0.970953886492654));
#11754=CARTESIAN_POINT('Ctrl Pts',(8.32325294445203,-0.527999999999998,
-0.970953886492654));
#11755=CARTESIAN_POINT('Ctrl Pts',(11.5219206080117,1.2,-0.983963678117389));
#11756=CARTESIAN_POINT('Ctrl Pts',(11.5219206080117,-0.527999999999998,
-0.983963678117389));
#11757=CARTESIAN_POINT('Ctrl Pts',(15.6615569014707,1.2,-1.18440486857005));
#11758=CARTESIAN_POINT('Ctrl Pts',(15.6615569014707,-0.527999999999998,
-1.18440486857005));
#11759=CARTESIAN_POINT('Ctrl Pts',(20.0374444881341,1.2,0.065252622484184));
#11760=CARTESIAN_POINT('Ctrl Pts',(20.0374444881341,-0.527999999999998,
0.065252622484184));
#11761=CARTESIAN_POINT('Ctrl Pts',(22.6903241895972,1.2,1.63809077991409));
#11762=CARTESIAN_POINT('Ctrl Pts',(22.6903241895972,-0.527999999999998,
1.63809077991409));
#11763=CARTESIAN_POINT('Ctrl Pts',(24.4689719714588,1.2,2.87083584760694));
#11764=CARTESIAN_POINT('Ctrl Pts',(24.4689719714588,-0.527999999999998,
2.87083584760694));
#11765=CARTESIAN_POINT('Ctrl Pts',(24.3083816239237,1.2,4.43315301466272));
#11766=CARTESIAN_POINT('Ctrl Pts',(24.3083816239237,-0.527999999999998,
4.43315301466272));
#11767=CARTESIAN_POINT('Ctrl Pts',(24.0522028467612,1.2,5.77390669222975));
#11768=CARTESIAN_POINT('Ctrl Pts',(24.0522028467612,-0.527999999999998,
5.77390669222975));
#11769=CARTESIAN_POINT('Ctrl Pts',(22.2137376328105,1.2,5.96195834426836));
#11770=CARTESIAN_POINT('Ctrl Pts',(22.2137376328105,-0.527999999999998,
5.96195834426836));
#11771=CARTESIAN_POINT('Ctrl Pts',(22.5278884970739,1.2,6.53446701068235));
#11772=CARTESIAN_POINT('Ctrl Pts',(22.5278884970739,-0.527999999999998,
6.53446701068235));
#11773=CARTESIAN_POINT('',(-28.2500418808543,0.,-2.07888836971769));
#11774=CARTESIAN_POINT('',(22.5278884970739,0.,6.53446701068235));
#11775=CARTESIAN_POINT('Ctrl Pts',(-28.2500418808543,0.,-2.07888836971769));
#11776=CARTESIAN_POINT('Ctrl Pts',(-27.9613439331009,0.,-1.81555449964671));
#11777=CARTESIAN_POINT('Ctrl Pts',(-27.180603234679,0.,-1.04385836116026));
#11778=CARTESIAN_POINT('Ctrl Pts',(-25.9983030006616,0.,-0.24124876693352));
#11779=CARTESIAN_POINT('Ctrl Pts',(-24.2346861695509,0.,-0.210983790359477));
#11780=CARTESIAN_POINT('Ctrl Pts',(-23.517870169039,0.,-1.68305705631707));
#11781=CARTESIAN_POINT('Ctrl Pts',(-23.2233109717715,0.,-3.05602157557454));
#11782=CARTESIAN_POINT('Ctrl Pts',(-22.1784263046757,0.,-3.93337248074442));
#11783=CARTESIAN_POINT('Ctrl Pts',(-19.19441431546,0.,-4.74815122044273));
#11784=CARTESIAN_POINT('Ctrl Pts',(-15.7509580358841,0.,-4.44216895895114));
#11785=CARTESIAN_POINT('Ctrl Pts',(-12.7021174144063,0.,-4.06331666259747));
#11786=CARTESIAN_POINT('Ctrl Pts',(-11.3962777017639,0.,-3.64648316501468));
#11787=CARTESIAN_POINT('Ctrl Pts',(-11.2344759364774,0.,-2.80455171594097));
#11788=CARTESIAN_POINT('Ctrl Pts',(-11.1732737269437,0.,-1.7662619507528));
#11789=CARTESIAN_POINT('Ctrl Pts',(-12.7612302838612,0.,-1.89361059761595));
#11790=CARTESIAN_POINT('Ctrl Pts',(-13.9972305202523,0.,-1.67844839769156));
#11791=CARTESIAN_POINT('Ctrl Pts',(-15.6400181726054,0.,-2.29491586659866));
#11792=CARTESIAN_POINT('Ctrl Pts',(-16.7051564115516,0.,0.0418535888021335));
#11793=CARTESIAN_POINT('Ctrl Pts',(-13.0664970088623,0.,0.88071809162054));
#11794=CARTESIAN_POINT('Ctrl Pts',(-10.5984973129989,0.,0.680667707785562));
#11795=CARTESIAN_POINT('Ctrl Pts',(-7.82942308877726,0.,0.695565326486597));
#11796=CARTESIAN_POINT('Ctrl Pts',(-6.07620266579566,0.,2.85997113365485));
#11797=CARTESIAN_POINT('Ctrl Pts',(-3.9066933893458,0.,4.14091208560258));
#11798=CARTESIAN_POINT('Ctrl Pts',(-2.0279101215411,0.,5.46819912841997));
#11799=CARTESIAN_POINT('Ctrl Pts',(0.00386116068497311,0.,5.86471136207473));
#11800=CARTESIAN_POINT('Ctrl Pts',(2.39576994688095,0.,5.73794061249253));
#11801=CARTESIAN_POINT('Ctrl Pts',(5.15590481840992,0.,5.78580883625202));
#11802=CARTESIAN_POINT('Ctrl Pts',(7.73518803149787,0.,5.79127386586831));
#11803=CARTESIAN_POINT('Ctrl Pts',(9.45734572072178,0.,4.67363967594622));
#11804=CARTESIAN_POINT('Ctrl Pts',(9.17706365495184,0.,2.96306509995752));
#11805=CARTESIAN_POINT('Ctrl Pts',(7.81796360098053,0.,3.18513163158631));
#11806=CARTESIAN_POINT('Ctrl Pts',(6.59699346312693,0.,3.38520430984983));
#11807=CARTESIAN_POINT('Ctrl Pts',(5.93021602745299,0.,1.85802575211607));
#11808=CARTESIAN_POINT('Ctrl Pts',(6.62071623580517,0.,0.188782666588939));
#11809=CARTESIAN_POINT('Ctrl Pts',(8.32325294445203,0.,-0.970953886492654));
#11810=CARTESIAN_POINT('Ctrl Pts',(11.5219206080117,0.,-0.983963678117389));
#11811=CARTESIAN_POINT('Ctrl Pts',(15.6615569014707,0.,-1.18440486857005));
#11812=CARTESIAN_POINT('Ctrl Pts',(20.0374444881341,0.,0.065252622484184));
#11813=CARTESIAN_POINT('Ctrl Pts',(22.6903241895972,0.,1.63809077991409));
#11814=CARTESIAN_POINT('Ctrl Pts',(24.4689719714588,0.,2.87083584760694));
#11815=CARTESIAN_POINT('Ctrl Pts',(24.3083816239237,0.,4.43315301466272));
#11816=CARTESIAN_POINT('Ctrl Pts',(24.0522028467612,0.,5.77390669222975));
#11817=CARTESIAN_POINT('Ctrl Pts',(22.2137376328105,0.,5.96195834426836));
#11818=CARTESIAN_POINT('Ctrl Pts',(22.5278884970739,0.,6.53446701068235));
#11819=CARTESIAN_POINT('',(22.5278884970739,1.2,6.53446701068235));
#11820=CARTESIAN_POINT('',(22.5278884970739,1.2,6.53446701068235));
#11821=CARTESIAN_POINT('',(-28.2500418808543,1.2,-2.07888836971769));
#11822=CARTESIAN_POINT('Ctrl Pts',(-28.2500418808543,1.2,-2.07888836971769));
#11823=CARTESIAN_POINT('Ctrl Pts',(-27.9613439331009,1.2,-1.81555449964671));
#11824=CARTESIAN_POINT('Ctrl Pts',(-27.180603234679,1.2,-1.04385836116026));
#11825=CARTESIAN_POINT('Ctrl Pts',(-25.9983030006616,1.2,-0.24124876693352));
#11826=CARTESIAN_POINT('Ctrl Pts',(-24.2346861695509,1.2,-0.210983790359477));
#11827=CARTESIAN_POINT('Ctrl Pts',(-23.517870169039,1.2,-1.68305705631707));
#11828=CARTESIAN_POINT('Ctrl Pts',(-23.2233109717715,1.2,-3.05602157557454));
#11829=CARTESIAN_POINT('Ctrl Pts',(-22.1784263046757,1.2,-3.93337248074442));
#11830=CARTESIAN_POINT('Ctrl Pts',(-19.19441431546,1.2,-4.74815122044273));
#11831=CARTESIAN_POINT('Ctrl Pts',(-15.7509580358841,1.2,-4.44216895895114));
#11832=CARTESIAN_POINT('Ctrl Pts',(-12.7021174144063,1.2,-4.06331666259747));
#11833=CARTESIAN_POINT('Ctrl Pts',(-11.3962777017639,1.2,-3.64648316501468));
#11834=CARTESIAN_POINT('Ctrl Pts',(-11.2344759364774,1.2,-2.80455171594097));
#11835=CARTESIAN_POINT('Ctrl Pts',(-11.1732737269437,1.2,-1.7662619507528));
#11836=CARTESIAN_POINT('Ctrl Pts',(-12.7612302838612,1.2,-1.89361059761595));
#11837=CARTESIAN_POINT('Ctrl Pts',(-13.9972305202523,1.2,-1.67844839769156));
#11838=CARTESIAN_POINT('Ctrl Pts',(-15.6400181726054,1.2,-2.29491586659866));
#11839=CARTESIAN_POINT('Ctrl Pts',(-16.7051564115516,1.2,0.0418535888021335));
#11840=CARTESIAN_POINT('Ctrl Pts',(-13.0664970088623,1.2,0.88071809162054));
#11841=CARTESIAN_POINT('Ctrl Pts',(-10.5984973129989,1.2,0.680667707785562));
#11842=CARTESIAN_POINT('Ctrl Pts',(-7.82942308877726,1.2,0.695565326486597));
#11843=CARTESIAN_POINT('Ctrl Pts',(-6.07620266579566,1.2,2.85997113365485));
#11844=CARTESIAN_POINT('Ctrl Pts',(-3.9066933893458,1.2,4.14091208560258));
#11845=CARTESIAN_POINT('Ctrl Pts',(-2.0279101215411,1.2,5.46819912841997));
#11846=CARTESIAN_POINT('Ctrl Pts',(0.00386116068497311,1.2,5.86471136207473));
#11847=CARTESIAN_POINT('Ctrl Pts',(2.39576994688095,1.2,5.73794061249253));
#11848=CARTESIAN_POINT('Ctrl Pts',(5.15590481840992,1.2,5.78580883625202));
#11849=CARTESIAN_POINT('Ctrl Pts',(7.73518803149787,1.2,5.79127386586831));
#11850=CARTESIAN_POINT('Ctrl Pts',(9.45734572072178,1.2,4.67363967594622));
#11851=CARTESIAN_POINT('Ctrl Pts',(9.17706365495184,1.2,2.96306509995752));
#11852=CARTESIAN_POINT('Ctrl Pts',(7.81796360098053,1.2,3.18513163158631));
#11853=CARTESIAN_POINT('Ctrl Pts',(6.59699346312693,1.2,3.38520430984983));
#11854=CARTESIAN_POINT('Ctrl Pts',(5.93021602745299,1.2,1.85802575211607));
#11855=CARTESIAN_POINT('Ctrl Pts',(6.62071623580517,1.2,0.188782666588939));
#11856=CARTESIAN_POINT('Ctrl Pts',(8.32325294445203,1.2,-0.970953886492654));
#11857=CARTESIAN_POINT('Ctrl Pts',(11.5219206080117,1.2,-0.983963678117389));
#11858=CARTESIAN_POINT('Ctrl Pts',(15.6615569014707,1.2,-1.18440486857005));
#11859=CARTESIAN_POINT('Ctrl Pts',(20.0374444881341,1.2,0.065252622484184));
#11860=CARTESIAN_POINT('Ctrl Pts',(22.6903241895972,1.2,1.63809077991409));
#11861=CARTESIAN_POINT('Ctrl Pts',(24.4689719714588,1.2,2.87083584760694));
#11862=CARTESIAN_POINT('Ctrl Pts',(24.3083816239237,1.2,4.43315301466272));
#11863=CARTESIAN_POINT('Ctrl Pts',(24.0522028467612,1.2,5.77390669222975));
#11864=CARTESIAN_POINT('Ctrl Pts',(22.2137376328105,1.2,5.96195834426836));
#11865=CARTESIAN_POINT('Ctrl Pts',(22.5278884970739,1.2,6.53446701068235));
#11866=CARTESIAN_POINT('',(-28.2500418808543,1.2,-2.07888836971769));
#11867=CARTESIAN_POINT('Ctrl Pts',(22.5278884970739,1.2,6.53446701068235));
#11868=CARTESIAN_POINT('Ctrl Pts',(22.5278884970739,-0.528,6.53446701068235));
#11869=CARTESIAN_POINT('Ctrl Pts',(23.1169295329987,1.2,7.60793564089319));
#11870=CARTESIAN_POINT('Ctrl Pts',(23.1169295329987,-0.528,7.60793564089319));
#11871=CARTESIAN_POINT('Ctrl Pts',(25.6536230216728,1.2,8.99671226634374));
#11872=CARTESIAN_POINT('Ctrl Pts',(25.6536230216728,-0.528,8.99671226634374));
#11873=CARTESIAN_POINT('Ctrl Pts',(28.6313409150419,1.2,7.38059742138985));
#11874=CARTESIAN_POINT('Ctrl Pts',(28.6313409150419,-0.528,7.38059742138985));
#11875=CARTESIAN_POINT('Ctrl Pts',(29.2791218831689,1.2,5.77930198399101));
#11876=CARTESIAN_POINT('Ctrl Pts',(29.2791218831689,-0.528,5.77930198399101));
#11877=CARTESIAN_POINT('',(29.2791218831689,0.,5.77930198399101));
#11878=CARTESIAN_POINT('Ctrl Pts',(22.5278884970739,0.,6.53446701068235));
#11879=CARTESIAN_POINT('Ctrl Pts',(24.0942932092593,0.,9.38908361325172));
#11880=CARTESIAN_POINT('Ctrl Pts',(28.2409339643995,0.,8.34567188259311));
#11881=CARTESIAN_POINT('Ctrl Pts',(29.2791218831689,0.,5.77930198399101));
#11882=CARTESIAN_POINT('',(29.2791218831689,1.2,5.77930198399101));
#11883=CARTESIAN_POINT('',(29.2791218831689,1.2,5.77930198399101));
#11884=CARTESIAN_POINT('Ctrl Pts',(22.5278884970739,1.2,6.53446701068235));
#11885=CARTESIAN_POINT('Ctrl Pts',(24.0942932092593,1.2,9.38908361325172));
#11886=CARTESIAN_POINT('Ctrl Pts',(28.2409339643995,1.2,8.34567188259311));
#11887=CARTESIAN_POINT('Ctrl Pts',(29.2791218831689,1.2,5.77930198399101));
#11888=CARTESIAN_POINT('Ctrl Pts',(29.2791218831689,1.2,5.77930198399101));
#11889=CARTESIAN_POINT('Ctrl Pts',(29.2791218831689,-0.528,5.77930198399101));
#11890=CARTESIAN_POINT('Ctrl Pts',(28.6578105275465,1.2,2.99017303105976));
#11891=CARTESIAN_POINT('Ctrl Pts',(28.6578105275465,-0.528,2.99017303105976));
#11892=CARTESIAN_POINT('Ctrl Pts',(27.094379352357,1.2,-0.177553803652863));
#11893=CARTESIAN_POINT('Ctrl Pts',(27.094379352357,-0.528,-0.177553803652863));
#11894=CARTESIAN_POINT('Ctrl Pts',(26.5382228845289,1.2,-7.0166851266602));
#11895=CARTESIAN_POINT('Ctrl Pts',(26.5382228845289,-0.528,-7.0166851266602));
#11896=CARTESIAN_POINT('Ctrl Pts',(24.629125296679,1.2,-6.94685713119016));
#11897=CARTESIAN_POINT('Ctrl Pts',(24.629125296679,-0.528,-6.94685713119016));
#11898=CARTESIAN_POINT('Ctrl Pts',(21.0225256793385,1.2,-7.04790997553116));
#11899=CARTESIAN_POINT('Ctrl Pts',(21.0225256793385,-0.528,-7.04790997553116));
#11900=CARTESIAN_POINT('',(21.0225256793385,0.,-7.04790997553116));
#11901=CARTESIAN_POINT('Ctrl Pts',(29.2791218831689,0.,5.77930198399101));
#11902=CARTESIAN_POINT('Ctrl Pts',(28.6578105275465,0.,2.99017303105976));
#11903=CARTESIAN_POINT('Ctrl Pts',(27.094379352357,0.,-0.177553803652863));
#11904=CARTESIAN_POINT('Ctrl Pts',(26.5382228845289,0.,-7.0166851266602));
#11905=CARTESIAN_POINT('Ctrl Pts',(24.629125296679,0.,-6.94685713119016));
#11906=CARTESIAN_POINT('Ctrl Pts',(21.0225256793385,0.,-7.04790997553116));
#11907=CARTESIAN_POINT('',(21.0225256793385,1.2,-7.04790997553116));
#11908=CARTESIAN_POINT('',(21.0225256793385,1.2,-7.04790997553116));
#11909=CARTESIAN_POINT('Ctrl Pts',(29.2791218831689,1.2,5.77930198399101));
#11910=CARTESIAN_POINT('Ctrl Pts',(28.6578105275465,1.2,2.99017303105976));
#11911=CARTESIAN_POINT('Ctrl Pts',(27.094379352357,1.2,-0.177553803652863));
#11912=CARTESIAN_POINT('Ctrl Pts',(26.5382228845289,1.2,-7.0166851266602));
#11913=CARTESIAN_POINT('Ctrl Pts',(24.629125296679,1.2,-6.94685713119016));
#11914=CARTESIAN_POINT('Ctrl Pts',(21.0225256793385,1.2,-7.04790997553116));
#11915=CARTESIAN_POINT('Ctrl Pts',(21.0225256793385,1.2,-7.04790997553116));
#11916=CARTESIAN_POINT('Ctrl Pts',(21.0225256793385,-0.528,-7.04790997553116));
#11917=CARTESIAN_POINT('Ctrl Pts',(19.8072013377325,1.2,-4.22629716477465));
#11918=CARTESIAN_POINT('Ctrl Pts',(19.8072013377325,-0.528,-4.22629716477465));
#11919=CARTESIAN_POINT('Ctrl Pts',(14.6387365156322,1.2,-3.68706222835893));
#11920=CARTESIAN_POINT('Ctrl Pts',(14.6387365156322,-0.528,-3.68706222835893));
#11921=CARTESIAN_POINT('Ctrl Pts',(9.29823038687031,1.2,-5.29769106666559));
#11922=CARTESIAN_POINT('Ctrl Pts',(9.29823038687031,-0.528,-5.29769106666559));
#11923=CARTESIAN_POINT('Ctrl Pts',(9.22738824529516,1.2,-8.22742371893551));
#11924=CARTESIAN_POINT('Ctrl Pts',(9.22738824529516,-0.528,-8.22742371893551));
#11925=CARTESIAN_POINT('',(9.22738824529516,0.,-8.22742371893551));
#11926=CARTESIAN_POINT('Ctrl Pts',(21.0225256793385,0.,-7.04790997553116));
#11927=CARTESIAN_POINT('Ctrl Pts',(19.8072013377325,0.,-4.22629716477465));
#11928=CARTESIAN_POINT('Ctrl Pts',(14.6387365156322,0.,-3.68706222835893));
#11929=CARTESIAN_POINT('Ctrl Pts',(9.29823038687031,0.,-5.29769106666559));
#11930=CARTESIAN_POINT('Ctrl Pts',(9.22738824529516,0.,-8.22742371893551));
#11931=CARTESIAN_POINT('',(9.22738824529516,1.2,-8.22742371893551));
#11932=CARTESIAN_POINT('',(9.22738824529516,1.2,-8.22742371893551));
#11933=CARTESIAN_POINT('Ctrl Pts',(21.0225256793385,1.2,-7.04790997553116));
#11934=CARTESIAN_POINT('Ctrl Pts',(19.8072013377325,1.2,-4.22629716477465));
#11935=CARTESIAN_POINT('Ctrl Pts',(14.6387365156322,1.2,-3.68706222835893));
#11936=CARTESIAN_POINT('Ctrl Pts',(9.29823038687031,1.2,-5.29769106666559));
#11937=CARTESIAN_POINT('Ctrl Pts',(9.22738824529516,1.2,-8.22742371893551));
#11938=CARTESIAN_POINT('Ctrl Pts',(9.22738824529516,1.2,-8.22742371893551));
#11939=CARTESIAN_POINT('Ctrl Pts',(9.22738824529516,-0.528,-8.22742371893551));
#11940=CARTESIAN_POINT('Ctrl Pts',(2.56764530386917,1.2,-8.25470956501187));
#11941=CARTESIAN_POINT('Ctrl Pts',(2.56764530386917,-0.528,-8.25470956501187));
#11942=CARTESIAN_POINT('Ctrl Pts',(-6.44753895416279,1.2,-9.5997804768992));
#11943=CARTESIAN_POINT('Ctrl Pts',(-6.44753895416279,-0.528,-9.5997804768992));
#11944=CARTESIAN_POINT('Ctrl Pts',(-18.1106375247657,1.2,-9.04522729065686));
#11945=CARTESIAN_POINT('Ctrl Pts',(-18.1106375247657,-0.528,-9.04522729065686));
#11946=CARTESIAN_POINT('Ctrl Pts',(-24.3161185416941,1.2,-8.46111575838443));
#11947=CARTESIAN_POINT('Ctrl Pts',(-24.3161185416941,-0.528,-8.46111575838443));
#11948=CARTESIAN_POINT('Ctrl Pts',(-28.8091126301565,1.2,-2.58884095234907));
#11949=CARTESIAN_POINT('Ctrl Pts',(-28.8091126301565,-0.528,-2.58884095234907));
#11950=CARTESIAN_POINT('Ctrl Pts',(-28.2500418808543,1.2,-2.07888836971769));
#11951=CARTESIAN_POINT('Ctrl Pts',(-28.2500418808543,-0.528,-2.07888836971769));
#11952=CARTESIAN_POINT('Ctrl Pts',(9.22738824529516,0.,-8.22742371893551));
#11953=CARTESIAN_POINT('Ctrl Pts',(2.56764530386917,0.,-8.25470956501187));
#11954=CARTESIAN_POINT('Ctrl Pts',(-6.44753895416279,0.,-9.5997804768992));
#11955=CARTESIAN_POINT('Ctrl Pts',(-18.1106375247657,0.,-9.04522729065686));
#11956=CARTESIAN_POINT('Ctrl Pts',(-24.3161185416941,0.,-8.46111575838443));
#11957=CARTESIAN_POINT('Ctrl Pts',(-28.8091126301565,0.,-2.58884095234907));
#11958=CARTESIAN_POINT('Ctrl Pts',(-28.2500418808543,0.,-2.07888836971769));
#11959=CARTESIAN_POINT('Ctrl Pts',(9.22738824529516,1.2,-8.22742371893551));
#11960=CARTESIAN_POINT('Ctrl Pts',(2.56764530386917,1.2,-8.25470956501187));
#11961=CARTESIAN_POINT('Ctrl Pts',(-6.44753895416279,1.2,-9.5997804768992));
#11962=CARTESIAN_POINT('Ctrl Pts',(-18.1106375247657,1.2,-9.04522729065686));
#11963=CARTESIAN_POINT('Ctrl Pts',(-24.3161185416941,1.2,-8.46111575838443));
#11964=CARTESIAN_POINT('Ctrl Pts',(-28.8091126301565,1.2,-2.58884095234907));
#11965=CARTESIAN_POINT('Ctrl Pts',(-28.2500418808543,1.2,-2.07888836971769));
#11966=CARTESIAN_POINT('Origin',(-2.41972159644388,1.2,5.11593538763785));
#11967=CARTESIAN_POINT('Origin',(-2.41972159644388,0.,5.11593538763785));
#11968=CARTESIAN_POINT('',(0.,0.,0.));
#11969=CARTESIAN_POINT('Origin',(-83.4892602927113,2.,28.6344795489034));
#11970=CARTESIAN_POINT('',(-83.4892602927113,2.,30.6344795489034));
#11971=CARTESIAN_POINT('',(-83.4892602927113,2.,26.6344795489034));
#11972=CARTESIAN_POINT('Origin',(-83.4892602927113,2.,28.6344795489034));
#11973=CARTESIAN_POINT('Origin',(-83.4892602927113,2.,28.6344795489034));
#11974=CARTESIAN_POINT('',(-83.4892602927113,2.5,26.1344795489034));
#11975=CARTESIAN_POINT('Origin',(-83.4892602927113,2.,26.1344795489034));
#11976=CARTESIAN_POINT('Origin',(-83.4892602927113,2.5,28.6344795489034));
#11977=CARTESIAN_POINT('Origin',(16.5107397072887,2.,28.6344795489026));
#11978=CARTESIAN_POINT('',(16.5107397072887,2.,30.6344795489026));
#11979=CARTESIAN_POINT('',(16.5107397072887,2.,26.6344795489026));
#11980=CARTESIAN_POINT('Origin',(16.5107397072887,2.,28.6344795489026));
#11981=CARTESIAN_POINT('Origin',(16.5107397072887,2.,28.6344795489026));
#11982=CARTESIAN_POINT('',(16.5107397072887,2.5,26.1344795489026));
#11983=CARTESIAN_POINT('Origin',(16.5107397072887,2.,26.1344795489026));
#11984=CARTESIAN_POINT('Origin',(16.5107397072887,2.5,28.6344795489026));
#11985=CARTESIAN_POINT('Origin',(16.5107397072887,2.5,28.6344795489026));
#11986=CARTESIAN_POINT('',(16.5107397072887,0.,30.6344795489026));
#11987=CARTESIAN_POINT('',(16.5107397072887,2.5,30.6344795489026));
#11988=CARTESIAN_POINT('Origin',(16.5107397072887,0.,28.6344795489026));
#11989=CARTESIAN_POINT('Origin',(-83.4892602927113,2.5,28.6344795489034));
#11990=CARTESIAN_POINT('',(-83.4892602927113,0.,30.6344795489034));
#11991=CARTESIAN_POINT('',(-83.4892602927113,2.5,30.6344795489034));
#11992=CARTESIAN_POINT('Origin',(-83.4892602927113,0.,28.6344795489034));
#11993=CARTESIAN_POINT('Origin',(16.5107397072887,2.5,28.6344795489026));
#11994=CARTESIAN_POINT('',(-83.4892602927114,2.49999999999999,16.8621786589128));
#11995=CARTESIAN_POINT('',(-83.4892602927112,2.5,40.406780438894));
#11996=CARTESIAN_POINT('Origin',(-83.4892602927113,2.5,28.6344795489034));
#11997=CARTESIAN_POINT('',(16.5107397072887,2.5,40.4067804388932));
#11998=CARTESIAN_POINT('',(16.5107397072887,2.5,40.4067804388932));
#11999=CARTESIAN_POINT('',(16.5107397072887,2.49999999999999,16.862178658912));
#12000=CARTESIAN_POINT('Origin',(16.5107397072887,2.5,28.6344795489026));
#12001=CARTESIAN_POINT('',(-83.4892602927114,2.49999999999999,16.8621786589128));
#12002=CARTESIAN_POINT('Origin',(16.5107397072887,0.,28.6344795489026));
#12003=CARTESIAN_POINT('',(16.5107397072887,-1.38777878078145E-14,40.9067804388932));
#12004=CARTESIAN_POINT('',(16.5107397072887,-1.38777878078145E-14,16.362178658912));
#12005=CARTESIAN_POINT('Origin',(16.5107397072887,0.,28.6344795489026));
#12006=CARTESIAN_POINT('',(-83.4892602927112,-1.38777878078145E-14,40.9067804388939));
#12007=CARTESIAN_POINT('',(16.5107397072887,-1.38777878078145E-14,40.9067804388932));
#12008=CARTESIAN_POINT('',(-83.4892602927114,-1.38777878078145E-14,16.3621786589128));
#12009=CARTESIAN_POINT('Origin',(-83.4892602927113,0.,28.6344795489034));
#12010=CARTESIAN_POINT('',(16.5107397072887,-1.38777878078145E-14,16.362178658912));
#12011=CARTESIAN_POINT('Origin',(16.5107397072887,2.5,28.6344795489026));
#12012=CARTESIAN_POINT('',(16.5107397072887,2.,16.362178658912));
#12013=CARTESIAN_POINT('',(16.5107397072887,2.5,16.362178658912));
#12014=CARTESIAN_POINT('',(16.5107397072887,2.,40.9067804388932));
#12015=CARTESIAN_POINT('Origin',(16.5107397072887,2.,28.6344795489026));
#12016=CARTESIAN_POINT('',(16.5107397072887,2.5,40.9067804388932));
#12017=CARTESIAN_POINT('Origin',(16.5107397072887,2.5,16.362178658912));
#12018=CARTESIAN_POINT('',(-83.4892602927114,2.,16.3621786589128));
#12019=CARTESIAN_POINT('',(-83.4892602927114,2.5,16.3621786589128));
#12020=CARTESIAN_POINT('',(16.5107397072887,2.,16.362178658912));
#12021=CARTESIAN_POINT('Origin',(-83.4892602927113,2.5,28.6344795489034));
#12022=CARTESIAN_POINT('',(-83.4892602927112,2.,40.9067804388939));
#12023=CARTESIAN_POINT('',(-83.4892602927112,2.5,40.906780438894));
#12024=CARTESIAN_POINT('Origin',(-83.4892602927113,2.,28.6344795489034));
#12025=CARTESIAN_POINT('Origin',(16.5107397072887,2.5,40.9067804388932));
#12026=CARTESIAN_POINT('',(-83.4892602927112,2.,40.9067804388939));
#12027=CARTESIAN_POINT('Origin',(16.5107397072886,2.,16.862178658912));
#12028=CARTESIAN_POINT('Origin',(16.5107397072887,2.,16.862178658912));
#12029=CARTESIAN_POINT('Origin',(-83.4892602927114,2.,16.8621786589128));
#12030=CARTESIAN_POINT('Origin',(-83.4892602927113,2.,28.6344795489034));
#12031=CARTESIAN_POINT('Origin',(-83.4892602927112,2.,40.4067804388939));
#12032=CARTESIAN_POINT('Origin',(16.5107397072887,2.,28.6344795489026));
#12033=CARTESIAN_POINT('Origin',(16.5107397072887,2.,40.4067804388932));
#12034=CARTESIAN_POINT('Origin',(16.5107397072888,2.,40.4067804388932));
#12035=CARTESIAN_POINT('',(0.,0.,0.));
#12036=CARTESIAN_POINT('Origin',(0.,0.,-0.5));
#12037=CARTESIAN_POINT('',(-3.5,-4.28626379701574E-16,-7.48223783394441E-32));
#12038=CARTESIAN_POINT('Origin',(0.,0.,0.));
#12039=CARTESIAN_POINT('',(-4.,-4.89858719658941E-16,-0.5));
#12040=CARTESIAN_POINT('Origin',(-3.5,-4.28626379701574E-16,-0.5));
#12041=CARTESIAN_POINT('Origin',(0.,0.,-0.5));
#12042=CARTESIAN_POINT('Origin',(0.,0.,-1.5));
#12043=CARTESIAN_POINT('',(-4.,-4.89858719658941E-16,-1.5));
#12044=CARTESIAN_POINT('Origin',(0.,0.,-1.5));
#12045=CARTESIAN_POINT('',(-3.5,-4.28626379701574E-16,-2.));
#12046=CARTESIAN_POINT('Origin',(-3.5,-4.28626379701574E-16,-1.5));
#12047=CARTESIAN_POINT('Origin',(0.,-6.93889390390723E-15,-2.));
#12048=CARTESIAN_POINT('Origin',(0.,0.,18.));
#12049=CARTESIAN_POINT('',(2.,-2.44929359829474E-16,0.));
#12050=CARTESIAN_POINT('Origin',(0.,0.,0.));
#12051=CARTESIAN_POINT('',(2.,-2.44929359829471E-16,18.));
#12052=CARTESIAN_POINT('',(2.,-2.44929359829471E-16,18.));
#12053=CARTESIAN_POINT('Origin',(0.,0.,18.));
#12054=CARTESIAN_POINT('Origin',(0.,-6.93889390390723E-15,-2.));
#12055=CARTESIAN_POINT('',(-4.,-7.42875262356617E-15,-2.));
#12056=CARTESIAN_POINT('Origin',(0.,-6.93889390390723E-15,-2.));
#12057=CARTESIAN_POINT('Origin',(0.,0.,0.));
#12058=CARTESIAN_POINT('Origin',(0.,0.,18.));
#12059=CARTESIAN_POINT('',(0.,0.,0.));
#12060=CARTESIAN_POINT('Origin',(72.6432649512037,1.5,-2.848178441575));
#12061=CARTESIAN_POINT('',(72.6432649512037,1.5,-0.848178441574995));
#12062=CARTESIAN_POINT('Origin',(72.6432649512037,1.5,-2.848178441575));
#12063=CARTESIAN_POINT('',(72.6432649512037,0.,-0.848178441574995));
#12064=CARTESIAN_POINT('',(72.6432649512037,1.5,-0.848178441575));
#12065=CARTESIAN_POINT('Origin',(72.6432649512037,0.,-2.848178441575));
#12066=CARTESIAN_POINT('Origin',(-27.3567350487966,1.5,-2.84817844157499));
#12067=CARTESIAN_POINT('',(-27.3567350487966,1.5,-0.848178441574983));
#12068=CARTESIAN_POINT('Origin',(-27.3567350487966,1.5,-2.84817844157499));
#12069=CARTESIAN_POINT('',(-27.3567350487966,0.,-0.848178441574983));
#12070=CARTESIAN_POINT('',(-27.3567350487966,1.5,-0.84817844157498));
#12071=CARTESIAN_POINT('Origin',(-27.3567350487966,0.,-2.84817844157499));
#12072=CARTESIAN_POINT('Origin',(72.6432649512037,1.5,-2.848178441575));
#12073=CARTESIAN_POINT('',(72.6432649512037,1.5,6.15182155842503));
#12074=CARTESIAN_POINT('',(72.6432649512038,1.5,-11.848178441575));
#12075=CARTESIAN_POINT('Origin',(72.6432649512037,1.5,-2.848178441575));
#12076=CARTESIAN_POINT('',(-27.3567350487966,1.5,-11.8481784415751));
#12077=CARTESIAN_POINT('',(72.6432649512038,1.5,-11.848178441575));
#12078=CARTESIAN_POINT('',(-27.3567350487967,1.5,6.15182155842505));
#12079=CARTESIAN_POINT('Origin',(-27.3567350487966,1.5,-2.84817844157499));
#12080=CARTESIAN_POINT('',(72.6432649512037,1.5,6.15182155842503));
#12081=CARTESIAN_POINT('Origin',(72.6432649512037,0.,-2.848178441575));
#12082=CARTESIAN_POINT('',(72.6432649512037,0.,6.15182155842503));
#12083=CARTESIAN_POINT('',(72.6432649512038,0.,-11.848178441575));
#12084=CARTESIAN_POINT('Origin',(72.6432649512037,0.,-2.848178441575));
#12085=CARTESIAN_POINT('',(-27.3567350487967,0.,6.15182155842505));
#12086=CARTESIAN_POINT('',(72.6432649512037,0.,6.15182155842503));
#12087=CARTESIAN_POINT('',(-27.3567350487966,0.,-11.8481784415751));
#12088=CARTESIAN_POINT('Origin',(-27.3567350487966,0.,-2.84817844157499));
#12089=CARTESIAN_POINT('',(72.6432649512038,0.,-11.848178441575));
#12090=CARTESIAN_POINT('Origin',(72.6432649512037,1.5,-2.848178441575));
#12091=CARTESIAN_POINT('',(72.6432649512038,1.5,-11.848178441575));
#12092=CARTESIAN_POINT('',(72.6432649512037,1.5,6.15182155842503));
#12093=CARTESIAN_POINT('Origin',(72.6432649512038,1.5,-11.848178441575));
#12094=CARTESIAN_POINT('',(-27.3567350487966,1.5,-11.8481784415751));
#12095=CARTESIAN_POINT('Origin',(-27.3567350487966,1.5,-2.84817844157499));
#12096=CARTESIAN_POINT('',(-27.3567350487967,1.5,6.15182155842505));
#12097=CARTESIAN_POINT('Origin',(72.6432649512037,1.5,6.15182155842503));
#12098=CARTESIAN_POINT('',(28.5850043251941,-1.90936729299665,-25.5986061084358));
#12099=CARTESIAN_POINT('',(-97.6574866258881,-3.40936729299665,5.99301234591294));
#12100=CARTESIAN_POINT('',(-54.9042559675172,0.590632707003351,3.03587344046757));
#12101=CARTESIAN_POINT('',(-27.5475209187207,-4.90936729299665,5.88405188204213));
#12102=CARTESIAN_POINT('',(-69.8551839372266,-6.40936729299665,23.8001364453098));
#12103=CARTESIAN_POINT('',(-79.4791391963444,-13.3636995291792,-25.8641584082518));
#12104=CARTESIAN_POINT('',(50.4233211750771,-14.4093672929975,-39.7687032930611));
#12105=CARTESIAN_POINT('',(65.4756374366101,-10.6093672929966,-7.7948390823764));
#12106=CARTESIAN_POINT('',(28.5850043251941,-14.4093672930043,31.6703529893693));
#12107=CARTESIAN_POINT('',(17.7390089836862,-7.90936729299665,0.187694998892024));
#12108=CARTESIAN_POINT('',(45.0957440324828,0.590632707003352,3.0358734404668));
#12109=CARTESIAN_POINT('',(-27.5475209187207,-10.6093672929966,5.88405188204213));
#12110=UNCERTAINTY_MEASURE_WITH_UNIT(LENGTH_MEASURE(0.01),#12138,
'DISTANCE_ACCURACY_VALUE',
'Maximum model space distance between geometric entities at asserted c
onnectivities');
#12111=UNCERTAINTY_MEASURE_WITH_UNIT(LENGTH_MEASURE(0.01),#12138,
'DISTANCE_ACCURACY_VALUE',
'Maximum model space distance between geometric entities at asserted c
onnectivities');
#12112=UNCERTAINTY_MEASURE_WITH_UNIT(LENGTH_MEASURE(0.01),#12138,
'DISTANCE_ACCURACY_VALUE',
'Maximum model space distance between geometric entities at asserted c
onnectivities');
#12113=UNCERTAINTY_MEASURE_WITH_UNIT(LENGTH_MEASURE(0.01),#12138,
'DISTANCE_ACCURACY_VALUE',
'Maximum model space distance between geometric entities at asserted c
onnectivities');
#12114=UNCERTAINTY_MEASURE_WITH_UNIT(LENGTH_MEASURE(0.01),#12138,
'DISTANCE_ACCURACY_VALUE',
'Maximum model space distance between geometric entities at asserted c
onnectivities');
#12115=UNCERTAINTY_MEASURE_WITH_UNIT(LENGTH_MEASURE(0.01),#12138,
'DISTANCE_ACCURACY_VALUE',
'Maximum model space distance between geometric entities at asserted c
onnectivities');
#12116=UNCERTAINTY_MEASURE_WITH_UNIT(LENGTH_MEASURE(0.01),#12138,
'DISTANCE_ACCURACY_VALUE',
'Maximum model space distance between geometric entities at asserted c
onnectivities');
#12117=UNCERTAINTY_MEASURE_WITH_UNIT(LENGTH_MEASURE(0.01),#12138,
'DISTANCE_ACCURACY_VALUE',
'Maximum model space distance between geometric entities at asserted c
onnectivities');
#12118=UNCERTAINTY_MEASURE_WITH_UNIT(LENGTH_MEASURE(0.01),#12138,
'DISTANCE_ACCURACY_VALUE',
'Maximum model space distance between geometric entities at asserted c
onnectivities');
#12119=UNCERTAINTY_MEASURE_WITH_UNIT(LENGTH_MEASURE(0.01),#12138,
'DISTANCE_ACCURACY_VALUE',
'Maximum model space distance between geometric entities at asserted c
onnectivities');
#12120=UNCERTAINTY_MEASURE_WITH_UNIT(LENGTH_MEASURE(0.01),#12138,
'DISTANCE_ACCURACY_VALUE',
'Maximum model space distance between geometric entities at asserted c
onnectivities');
#12121=UNCERTAINTY_MEASURE_WITH_UNIT(LENGTH_MEASURE(0.01),#12138,
'DISTANCE_ACCURACY_VALUE',
'Maximum model space distance between geometric entities at asserted c
onnectivities');
#12122=UNCERTAINTY_MEASURE_WITH_UNIT(LENGTH_MEASURE(0.01),#12138,
'DISTANCE_ACCURACY_VALUE',
'Maximum model space distance between geometric entities at asserted c
onnectivities');
#12123=UNCERTAINTY_MEASURE_WITH_UNIT(LENGTH_MEASURE(0.01),#12138,
'DISTANCE_ACCURACY_VALUE',
'Maximum model space distance between geometric entities at asserted c
onnectivities');
#12124=(
GEOMETRIC_REPRESENTATION_CONTEXT(3)
GLOBAL_UNCERTAINTY_ASSIGNED_CONTEXT((#12110))
GLOBAL_UNIT_ASSIGNED_CONTEXT((#12138,#12140,#12141))
REPRESENTATION_CONTEXT('','3D')
);
#12125=(
GEOMETRIC_REPRESENTATION_CONTEXT(3)
GLOBAL_UNCERTAINTY_ASSIGNED_CONTEXT((#12111))
GLOBAL_UNIT_ASSIGNED_CONTEXT((#12138,#12140,#12141))
REPRESENTATION_CONTEXT('','3D')
);
#12126=(
GEOMETRIC_REPRESENTATION_CONTEXT(3)
GLOBAL_UNCERTAINTY_ASSIGNED_CONTEXT((#12112))
GLOBAL_UNIT_ASSIGNED_CONTEXT((#12138,#12140,#12141))
REPRESENTATION_CONTEXT('','3D')
);
#12127=(
GEOMETRIC_REPRESENTATION_CONTEXT(3)
GLOBAL_UNCERTAINTY_ASSIGNED_CONTEXT((#12113))
GLOBAL_UNIT_ASSIGNED_CONTEXT((#12138,#12140,#12141))
REPRESENTATION_CONTEXT('','3D')
);
#12128=(
GEOMETRIC_REPRESENTATION_CONTEXT(3)
GLOBAL_UNCERTAINTY_ASSIGNED_CONTEXT((#12114))
GLOBAL_UNIT_ASSIGNED_CONTEXT((#12138,#12140,#12141))
REPRESENTATION_CONTEXT('','3D')
);
#12129=(
GEOMETRIC_REPRESENTATION_CONTEXT(3)
GLOBAL_UNCERTAINTY_ASSIGNED_CONTEXT((#12115))
GLOBAL_UNIT_ASSIGNED_CONTEXT((#12138,#12140,#12141))
REPRESENTATION_CONTEXT('','3D')
);
#12130=(
GEOMETRIC_REPRESENTATION_CONTEXT(3)
GLOBAL_UNCERTAINTY_ASSIGNED_CONTEXT((#12116))
GLOBAL_UNIT_ASSIGNED_CONTEXT((#12138,#12140,#12141))
REPRESENTATION_CONTEXT('','3D')
);
#12131=(
GEOMETRIC_REPRESENTATION_CONTEXT(3)
GLOBAL_UNCERTAINTY_ASSIGNED_CONTEXT((#12117))
GLOBAL_UNIT_ASSIGNED_CONTEXT((#12138,#12140,#12141))
REPRESENTATION_CONTEXT('','3D')
);
#12132=(
GEOMETRIC_REPRESENTATION_CONTEXT(3)
GLOBAL_UNCERTAINTY_ASSIGNED_CONTEXT((#12118))
GLOBAL_UNIT_ASSIGNED_CONTEXT((#12138,#12140,#12141))
REPRESENTATION_CONTEXT('','3D')
);
#12133=(
GEOMETRIC_REPRESENTATION_CONTEXT(3)
GLOBAL_UNCERTAINTY_ASSIGNED_CONTEXT((#12119))
GLOBAL_UNIT_ASSIGNED_CONTEXT((#12138,#12140,#12141))
REPRESENTATION_CONTEXT('','3D')
);
#12134=(
GEOMETRIC_REPRESENTATION_CONTEXT(3)
GLOBAL_UNCERTAINTY_ASSIGNED_CONTEXT((#12120))
GLOBAL_UNIT_ASSIGNED_CONTEXT((#12138,#12140,#12141))
REPRESENTATION_CONTEXT('','3D')
);
#12135=(
GEOMETRIC_REPRESENTATION_CONTEXT(3)
GLOBAL_UNCERTAINTY_ASSIGNED_CONTEXT((#12121))
GLOBAL_UNIT_ASSIGNED_CONTEXT((#12138,#12140,#12141))
REPRESENTATION_CONTEXT('','3D')
);
#12136=(
GEOMETRIC_REPRESENTATION_CONTEXT(3)
GLOBAL_UNCERTAINTY_ASSIGNED_CONTEXT((#12122))
GLOBAL_UNIT_ASSIGNED_CONTEXT((#12138,#12140,#12141))
REPRESENTATION_CONTEXT('','3D')
);
#12137=(
GEOMETRIC_REPRESENTATION_CONTEXT(3)
GLOBAL_UNCERTAINTY_ASSIGNED_CONTEXT((#12123))
GLOBAL_UNIT_ASSIGNED_CONTEXT((#12138,#12140,#12141))
REPRESENTATION_CONTEXT('','3D')
);
#12138=(
LENGTH_UNIT()
NAMED_UNIT(*)
SI_UNIT(.MILLI.,.METRE.)
);
#12139=(
LENGTH_UNIT()
NAMED_UNIT(*)
SI_UNIT($,.METRE.)
);
#12140=(
NAMED_UNIT(*)
PLANE_ANGLE_UNIT()
SI_UNIT($,.RADIAN.)
);
#12141=(
NAMED_UNIT(*)
SI_UNIT($,.STERADIAN.)
SOLID_ANGLE_UNIT()
);
#12142=SHAPE_DEFINITION_REPRESENTATION(#12155,#12183);
#12143=SHAPE_DEFINITION_REPRESENTATION(#12156,#12184);
#12144=SHAPE_DEFINITION_REPRESENTATION(#12157,#12185);
#12145=SHAPE_DEFINITION_REPRESENTATION(#12158,#12186);
#12146=SHAPE_DEFINITION_REPRESENTATION(#12159,#12187);
#12147=SHAPE_DEFINITION_REPRESENTATION(#12160,#12188);
#12148=SHAPE_DEFINITION_REPRESENTATION(#12161,#12189);
#12149=SHAPE_DEFINITION_REPRESENTATION(#12162,#12190);
#12150=SHAPE_DEFINITION_REPRESENTATION(#12166,#12191);
#12151=SHAPE_DEFINITION_REPRESENTATION(#12167,#12192);
#12152=SHAPE_DEFINITION_REPRESENTATION(#12168,#12193);
#12153=SHAPE_DEFINITION_REPRESENTATION(#12169,#12194);
#12154=SHAPE_DEFINITION_REPRESENTATION(#12170,#12195);
#12155=PRODUCT_DEFINITION_SHAPE('',$,#12197);
#12156=PRODUCT_DEFINITION_SHAPE('',$,#12198);
#12157=PRODUCT_DEFINITION_SHAPE('',$,#12199);
#12158=PRODUCT_DEFINITION_SHAPE('',$,#12200);
#12159=PRODUCT_DEFINITION_SHAPE('',$,#12201);
#12160=PRODUCT_DEFINITION_SHAPE('',$,#12202);
#12161=PRODUCT_DEFINITION_SHAPE('',$,#12203);
#12162=PRODUCT_DEFINITION_SHAPE('',$,#12204);
#12163=PRODUCT_DEFINITION_SHAPE($,$,#66);
#12164=PRODUCT_DEFINITION_SHAPE($,$,#67);
#12165=PRODUCT_DEFINITION_SHAPE($,$,#68);
#12166=PRODUCT_DEFINITION_SHAPE('',$,#12205);
#12167=PRODUCT_DEFINITION_SHAPE('',$,#12206);
#12168=PRODUCT_DEFINITION_SHAPE('',$,#12207);
#12169=PRODUCT_DEFINITION_SHAPE('',$,#12208);
#12170=PRODUCT_DEFINITION_SHAPE('',$,#12209);
#12171=PRODUCT_DEFINITION_SHAPE($,$,#69);
#12172=PRODUCT_DEFINITION_SHAPE($,$,#70);
#12173=PRODUCT_DEFINITION_SHAPE($,$,#71);
#12174=PRODUCT_DEFINITION_SHAPE($,$,#72);
#12175=PRODUCT_DEFINITION_SHAPE($,$,#73);
#12176=PRODUCT_DEFINITION_SHAPE($,$,#74);
#12177=PRODUCT_DEFINITION_SHAPE($,$,#75);
#12178=PRODUCT_DEFINITION_SHAPE($,$,#76);
#12179=PRODUCT_DEFINITION_SHAPE($,$,#77);
#12180=PRODUCT_DEFINITION_SHAPE($,$,#78);
#12181=PRODUCT_DEFINITION_SHAPE($,$,#79);
#12182=PRODUCT_DEFINITION_SHAPE($,$,#80);
#12183=SHAPE_REPRESENTATION('',(#1961,#2148,#2149,#2150,#2151,#2152,#2153,
#2154,#2155,#2156,#2157,#2158,#2159),#12124);
#12184=SHAPE_REPRESENTATION('',(#1962),#12125);
#12185=SHAPE_REPRESENTATION('',(#1997),#12126);
#12186=SHAPE_REPRESENTATION('',(#2005),#12127);
#12187=SHAPE_REPRESENTATION('',(#2013,#2046,#2047,#2048),#12128);
#12188=SHAPE_REPRESENTATION('',(#2014),#12129);
#12189=SHAPE_REPRESENTATION('',(#2022),#12130);
#12190=SHAPE_REPRESENTATION('',(#2036),#12131);
#12191=SHAPE_REPRESENTATION('',(#2049),#12132);
#12192=SHAPE_REPRESENTATION('',(#2074),#12133);
#12193=SHAPE_REPRESENTATION('',(#2080),#12134);
#12194=SHAPE_REPRESENTATION('',(#2115),#12135);
#12195=SHAPE_REPRESENTATION('',(#2131),#12136);
#12196=PRODUCT_DEFINITION_CONTEXT('part definition',#12237,'design');
#12197=PRODUCT_DEFINITION('2026-11-08-21-39-50-231','MAS-150',#12210,#12196);
#12198=PRODUCT_DEFINITION('cover 2','Front Cover',#12211,#12196);
#12199=PRODUCT_DEFINITION('knife','knife',#12212,#12196);
#12200=PRODUCT_DEFINITION('knife smal','Knife small',#12213,#12196);
#12201=PRODUCT_DEFINITION('Scissors','Scissors',#12214,#12196);
#12202=PRODUCT_DEFINITION('casy 1','Blade_1',#12215,#12196);
#12203=PRODUCT_DEFINITION('casy 2','Blade_2',#12216,#12196);
#12204=PRODUCT_DEFINITION('small pin','small pin',#12217,#12196);
#12205=PRODUCT_DEFINITION('Corkscrew','Corkscrew',#12218,#12196);
#12206=PRODUCT_DEFINITION('Bottol opener','Bottle opener',#12219,#12196);
#12207=PRODUCT_DEFINITION('cover','Back cover',#12220,#12196);
#12208=PRODUCT_DEFINITION('Big pin','Big pin',#12221,#12196);
#12209=PRODUCT_DEFINITION('Pivot spechinf','Pivot spacer',#12222,#12196);
#12210=PRODUCT_DEFINITION_FORMATION('',$,#12239);
#12211=PRODUCT_DEFINITION_FORMATION('',$,#12240);
#12212=PRODUCT_DEFINITION_FORMATION('',$,#12241);
#12213=PRODUCT_DEFINITION_FORMATION('',$,#12242);
#12214=PRODUCT_DEFINITION_FORMATION('',$,#12243);
#12215=PRODUCT_DEFINITION_FORMATION('',$,#12244);
#12216=PRODUCT_DEFINITION_FORMATION('',$,#12245);
#12217=PRODUCT_DEFINITION_FORMATION('',$,#12246);
#12218=PRODUCT_DEFINITION_FORMATION('',$,#12247);
#12219=PRODUCT_DEFINITION_FORMATION('',$,#12248);
#12220=PRODUCT_DEFINITION_FORMATION('',$,#12249);
#12221=PRODUCT_DEFINITION_FORMATION('',$,#12250);
#12222=PRODUCT_DEFINITION_FORMATION('',$,#12251);
#12223=PRODUCT_RELATED_PRODUCT_CATEGORY('MAS-150','MAS-150',(#12239));
#12224=PRODUCT_RELATED_PRODUCT_CATEGORY('Front Cover','Front Cover',(#12240));
#12225=PRODUCT_RELATED_PRODUCT_CATEGORY('knife','knife',(#12241));
#12226=PRODUCT_RELATED_PRODUCT_CATEGORY('Knife small','Knife small',(#12242));
#12227=PRODUCT_RELATED_PRODUCT_CATEGORY('Scissors','Scissors',(#12243));
#12228=PRODUCT_RELATED_PRODUCT_CATEGORY('Blade_1','Blade_1',(#12244));
#12229=PRODUCT_RELATED_PRODUCT_CATEGORY('Blade_2','Blade_2',(#12245));
#12230=PRODUCT_RELATED_PRODUCT_CATEGORY('small pin','small pin',(#12246));
#12231=PRODUCT_RELATED_PRODUCT_CATEGORY('Corkscrew','Corkscrew',(#12247));
#12232=PRODUCT_RELATED_PRODUCT_CATEGORY('Bottle opener','Bottle opener',
(#12248));
#12233=PRODUCT_RELATED_PRODUCT_CATEGORY('Back cover','Back cover',(#12249));
#12234=PRODUCT_RELATED_PRODUCT_CATEGORY('Big pin','Big pin',(#12250));
#12235=PRODUCT_RELATED_PRODUCT_CATEGORY('Pivot spacer','Pivot spacer',(#12251));
#12236=APPLICATION_PROTOCOL_DEFINITION('international standard',
'automotive_design',2009,#12237);
#12237=APPLICATION_CONTEXT(
'Core Data for Automotive Mechanical Design Process');
#12238=PRODUCT_CONTEXT('part definition',#12237,'mechanical');
#12239=PRODUCT('2026-11-08-21-39-50-231','MAS-150','STEP AP203',(#12238));
#12240=PRODUCT('cover 2','Front Cover',$,(#12238));
#12241=PRODUCT('knife','knife',$,(#12238));
#12242=PRODUCT('knife smal','Knife small',$,(#12238));
#12243=PRODUCT('Scissors','Scissors',$,(#12238));
#12244=PRODUCT('casy 1','Blade_1',$,(#12238));
#12245=PRODUCT('casy 2','Blade_2',$,(#12238));
#12246=PRODUCT('small pin','small pin',$,(#12238));
#12247=PRODUCT('Corkscrew','Corkscrew',$,(#12238));
#12248=PRODUCT('Bottol opener','Bottle opener',$,(#12238));
#12249=PRODUCT('cover','Back cover',$,(#12238));
#12250=PRODUCT('Big pin','Big pin',$,(#12238));
#12251=PRODUCT('Pivot spechinf','Pivot spacer',$,(#12238));
#12252=PRESENTATION_STYLE_ASSIGNMENT((#12254));
#12253=PRESENTATION_STYLE_ASSIGNMENT((#12255));
#12254=SURFACE_STYLE_USAGE(.BOTH.,#12256);
#12255=SURFACE_STYLE_USAGE(.BOTH.,#12257);
#12256=SURFACE_SIDE_STYLE('',(#12258));
#12257=SURFACE_SIDE_STYLE('',(#12259));
#12258=SURFACE_STYLE_FILL_AREA(#12260);
#12259=SURFACE_STYLE_FILL_AREA(#12261);
#12260=FILL_AREA_STYLE('Steel - Satin',(#12262));
#12261=FILL_AREA_STYLE('Opaque(23,69,131)',(#12263));
#12262=FILL_AREA_STYLE_COLOUR('Steel - Satin',#12264);
#12263=FILL_AREA_STYLE_COLOUR('Opaque(23,69,131)',#12265);
#12264=COLOUR_RGB('Steel - Satin',0.627450980392157,0.627450980392157,0.627450980392157);
#12265=COLOUR_RGB('Opaque(23,69,131)',0.0901960784313725,0.270588235294118,
0.513725490196078);
ENDSEC;
END-ISO-10303-21;
